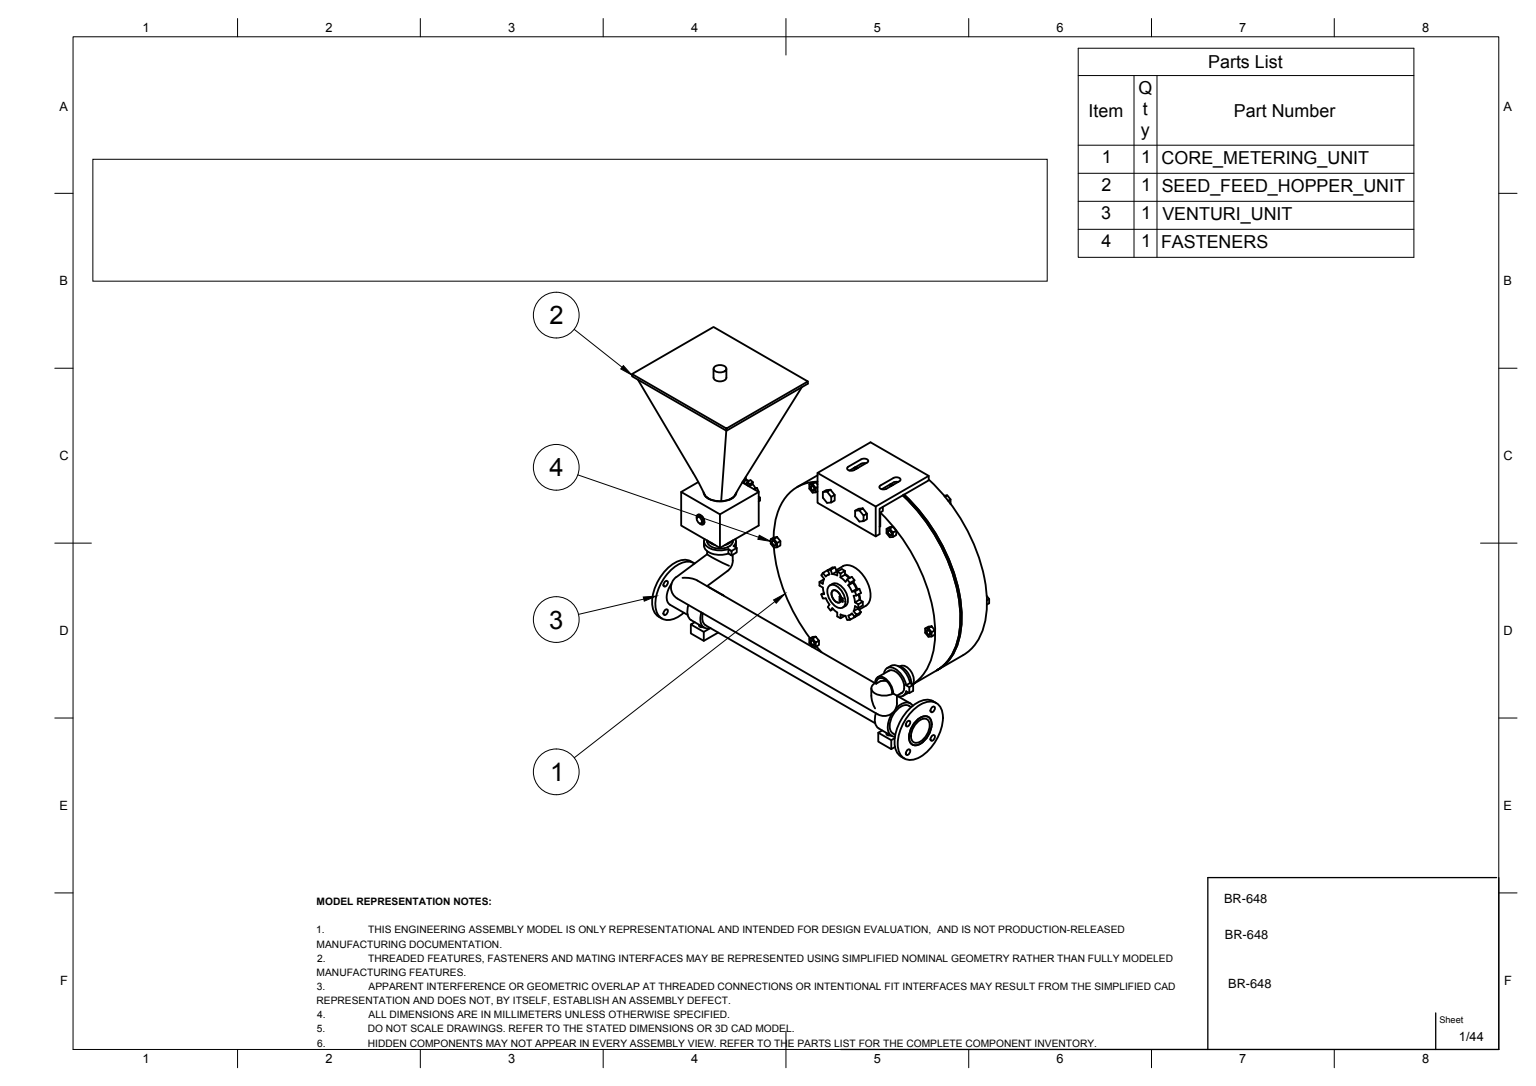
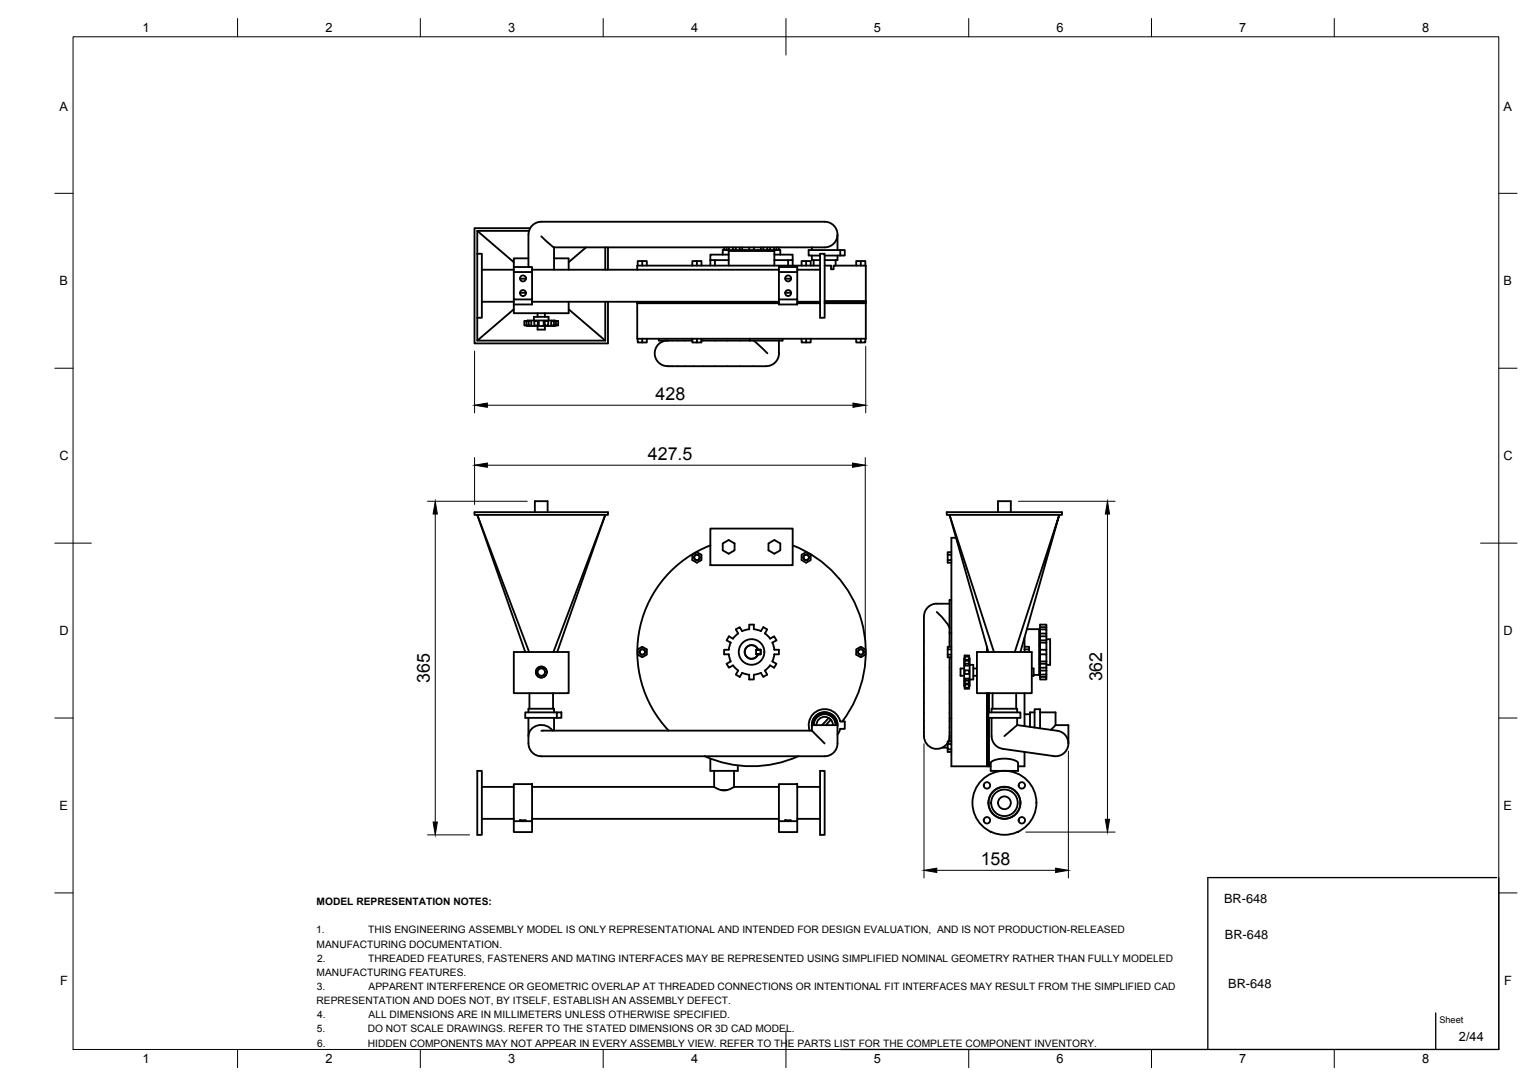
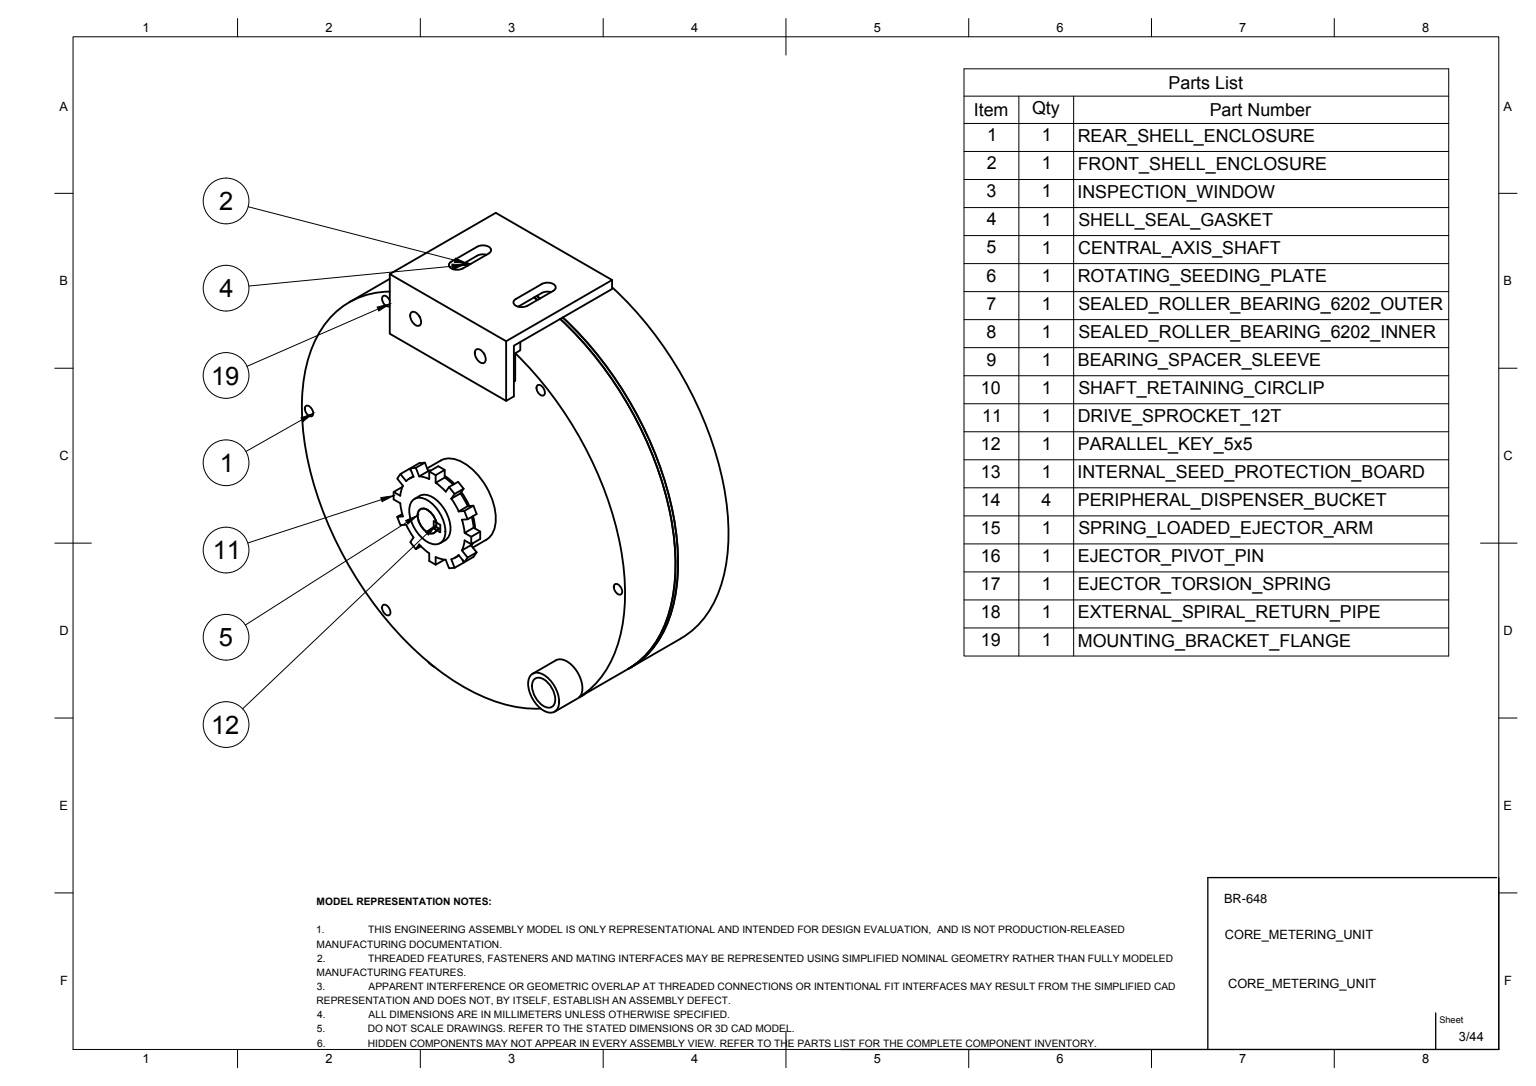
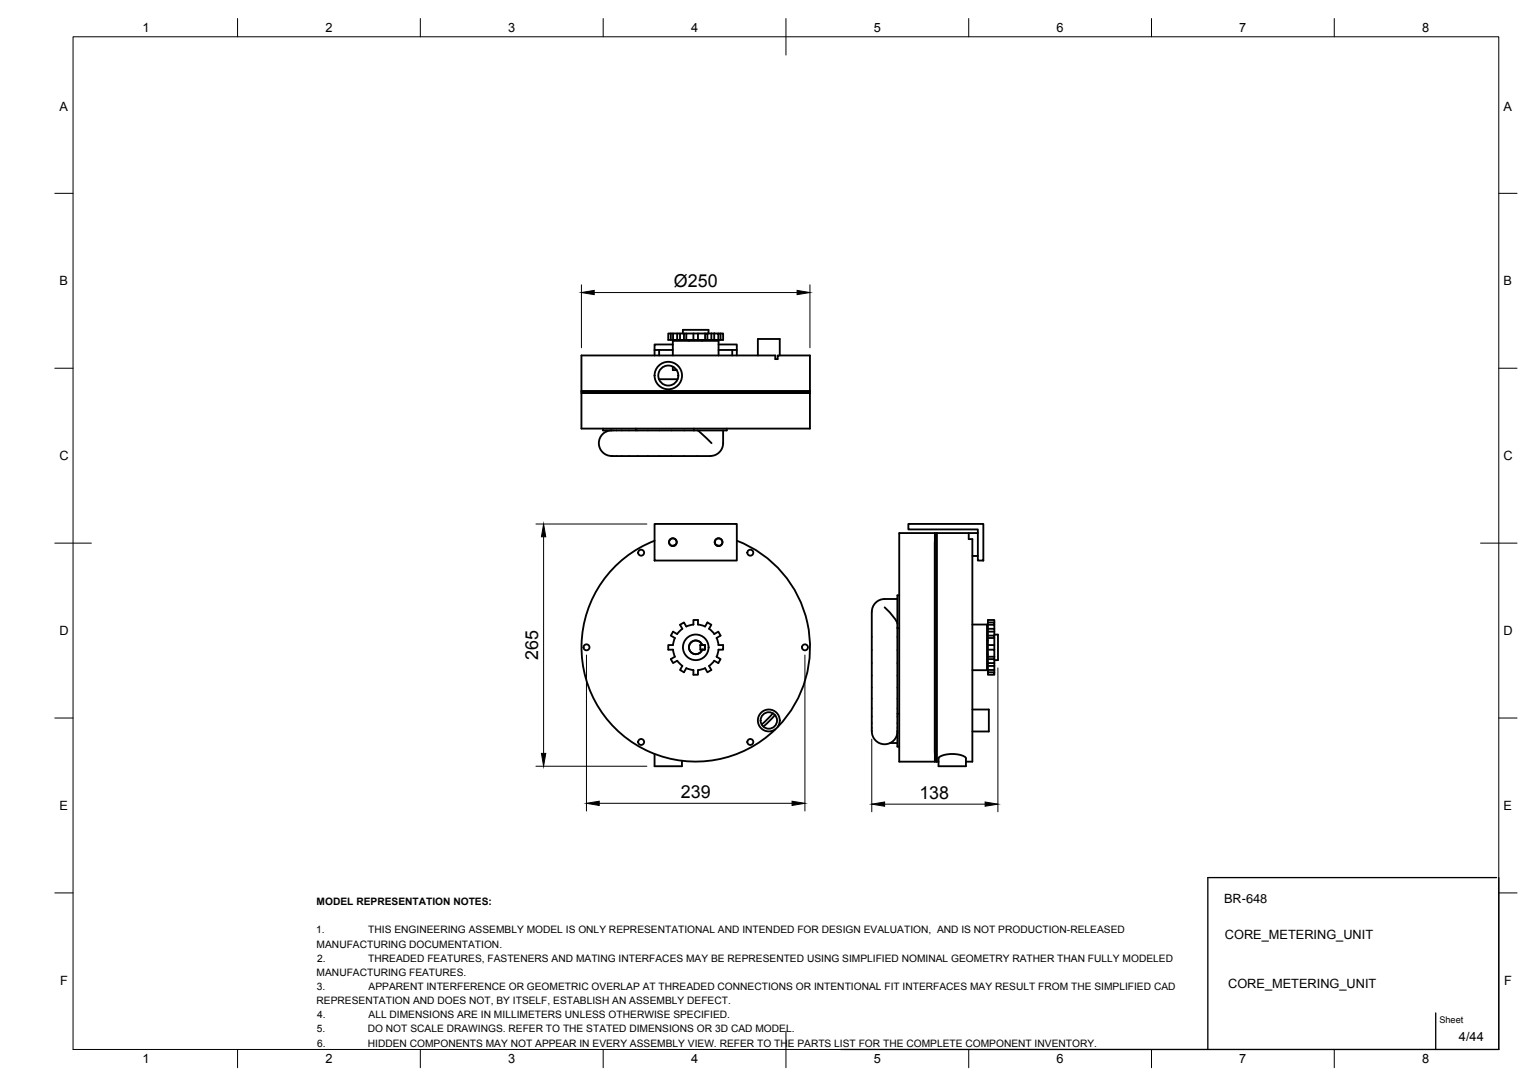
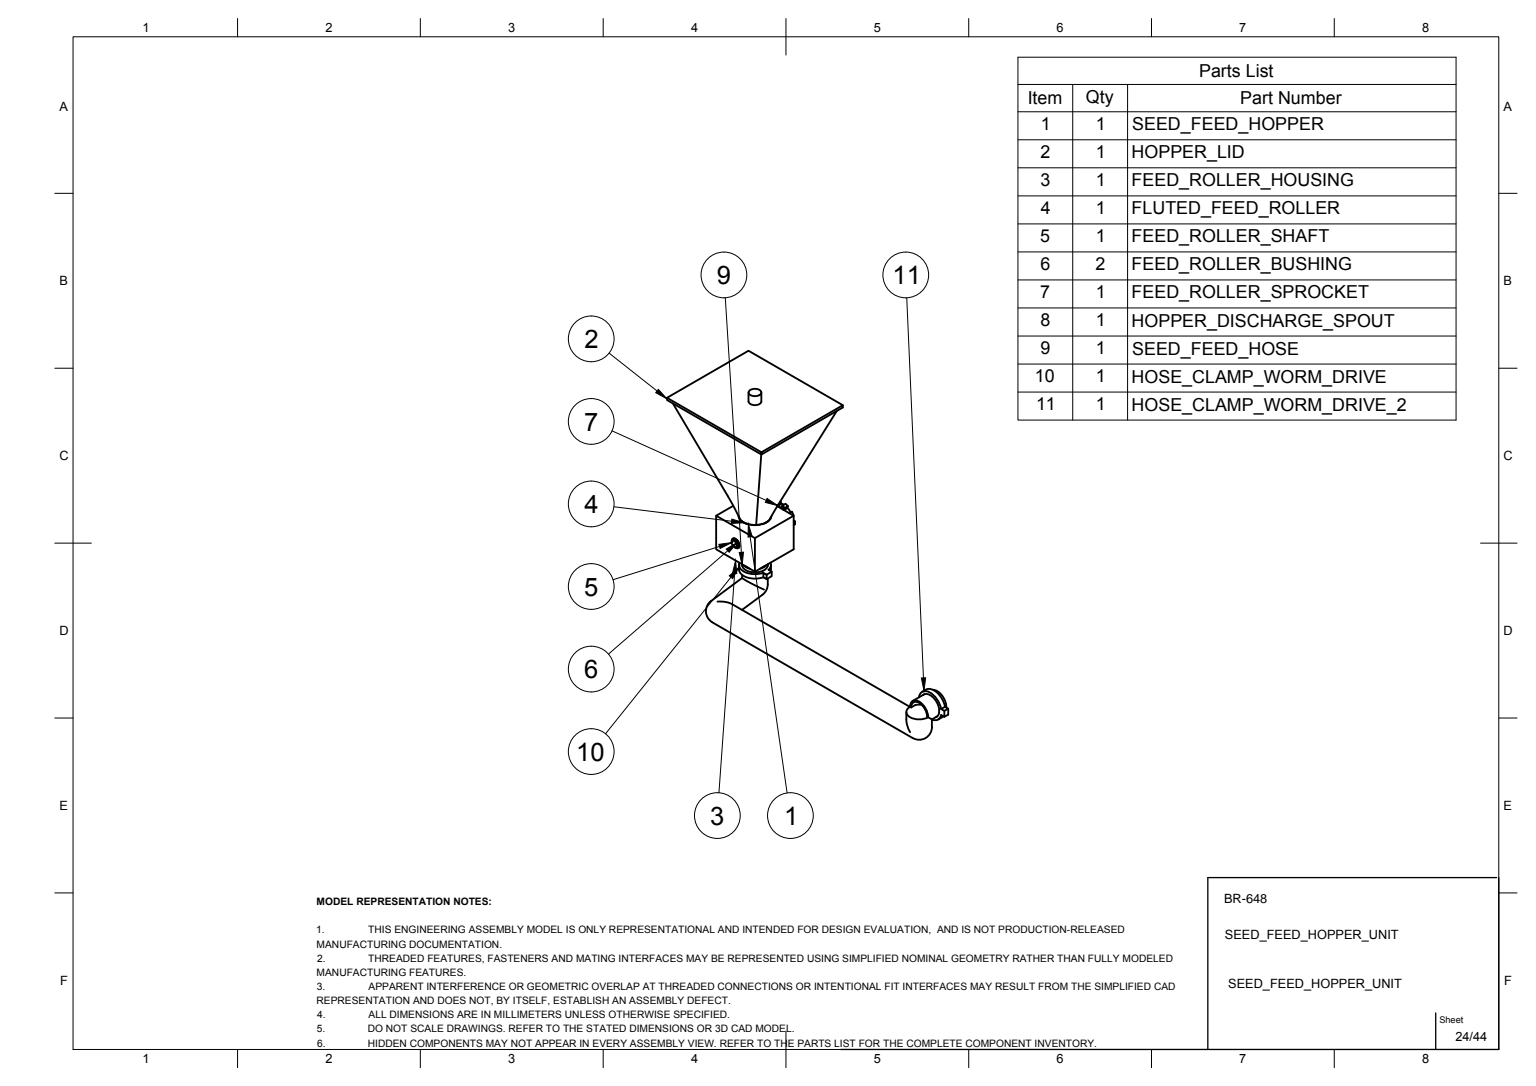
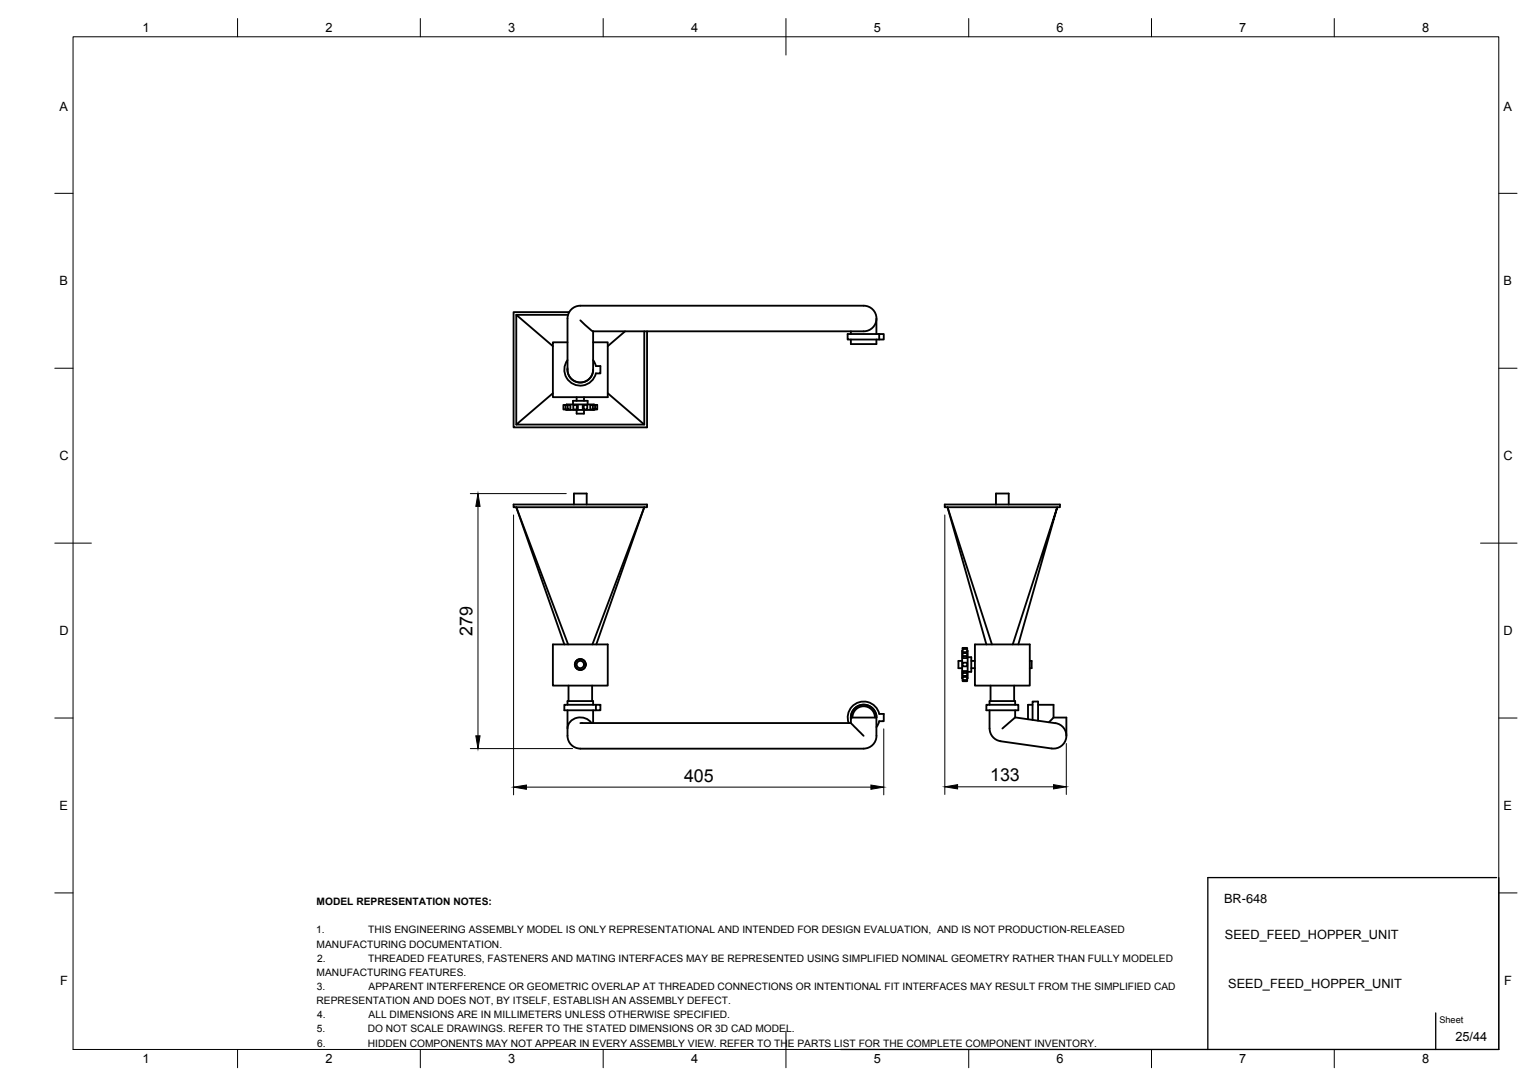
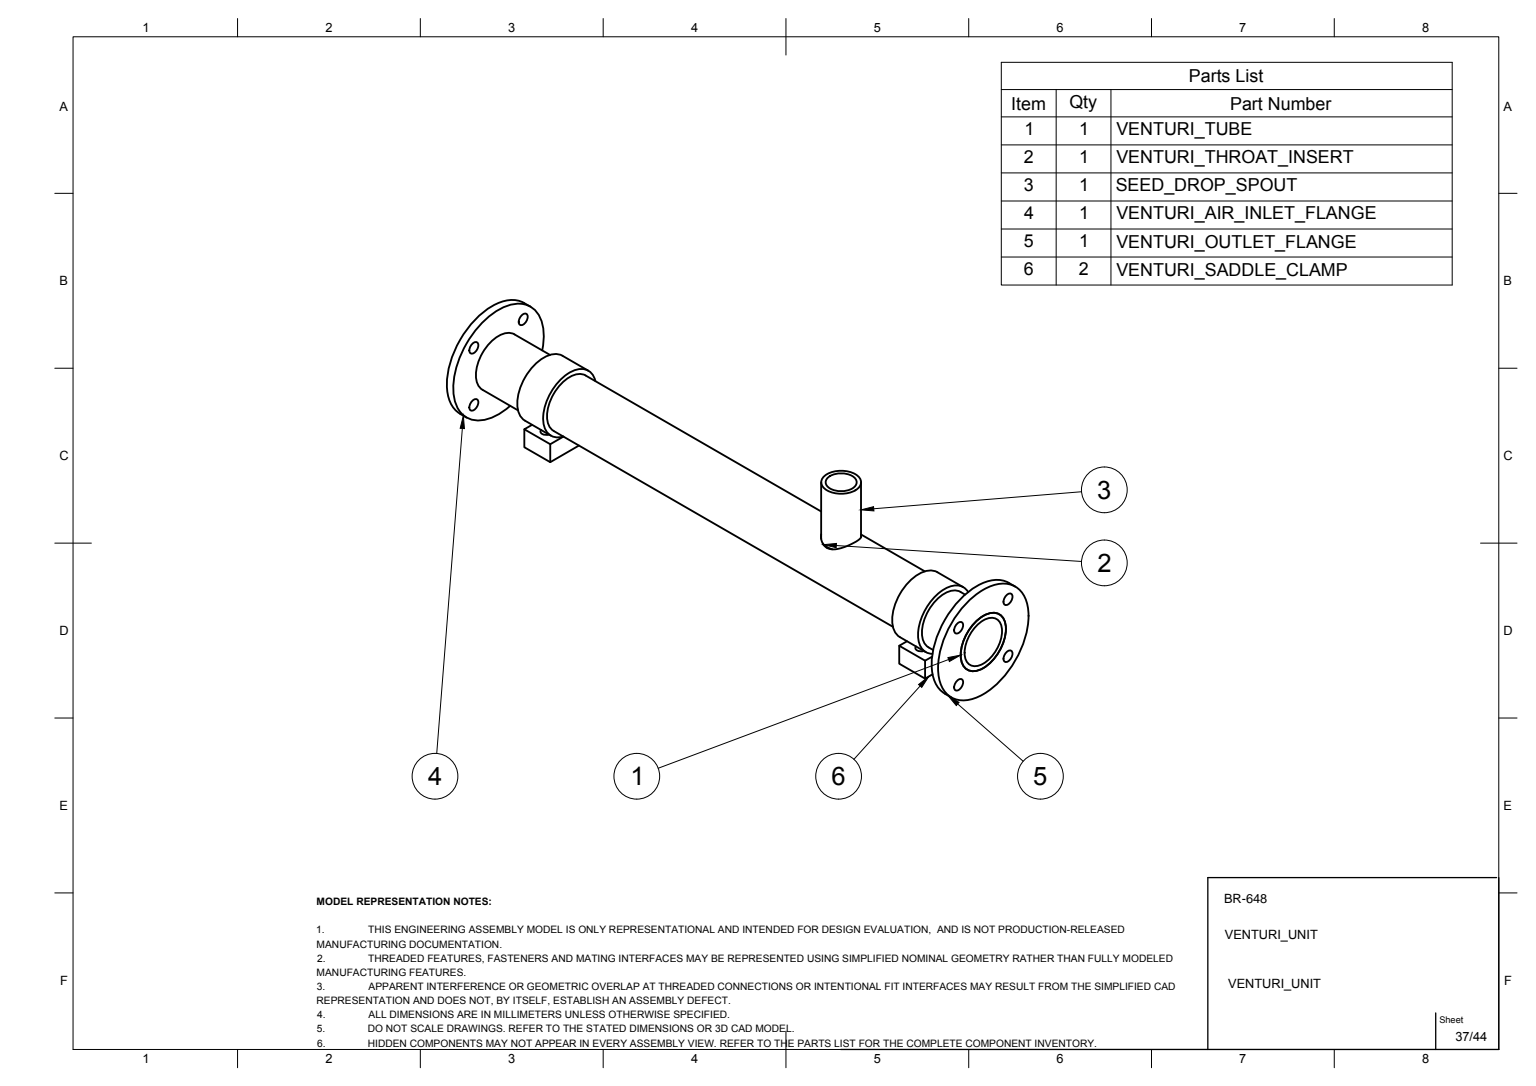
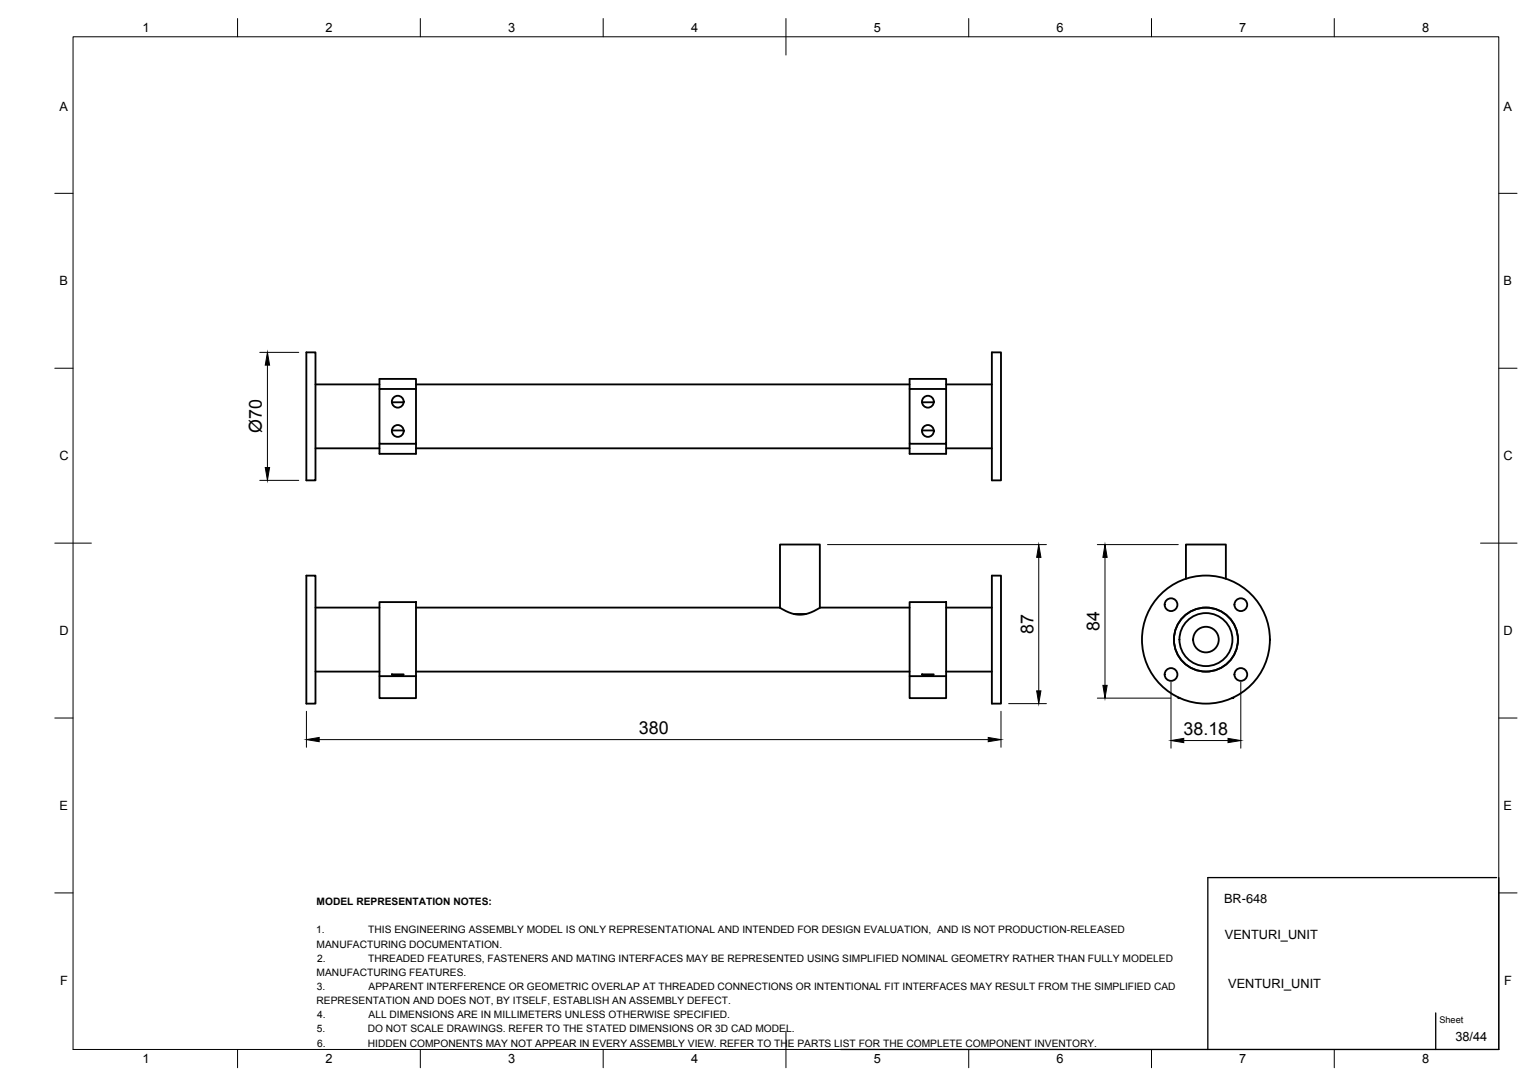
ISO-10303-21;
HEADER;
FILE_DESCRIPTION((''),'2;1');
FILE_NAME('BR-648','2026-10-01T22:05:39-07:00',(''),(''),'','','');
FILE_SCHEMA (('AUTOMOTIVE_DESIGN { 1 0 10303 214 3 1 1 }'));
ENDSEC;
DATA;
#10 = MECHANICAL_DESIGN_GEOMETRIC_PRESENTATION_REPRESENTATION('',(#605,#606,
#607,#608,#609,#610,#611,#612,#613,#614,#615,#616,#617,#618,#619,#620,#621,
#622,#623,#624,#625,#626,#627,#628,#629,#630,#631,#632,#633,#634,#635,#636,
#637,#638,#639,#640,#641,#642,#643,#644,#645,#646),#24628) ;
#11 = CONICAL_SURFACE('',#15204,1.225,0.221314442347791) ;
#12 = CONICAL_SURFACE('',#15210,1.225,0.221314442347791) ;
#13 = B_SPLINE_SURFACE_WITH_KNOTS('',3,3,((#22362,#22363,#22364,#22365,#22366,
#22367,#22368),(#22369,#22370,#22371,#22372,#22373,#22374,#22375),(#22376,
#22377,#22378,#22379,#22380,#22381,#22382),(#22383,#22384,#22385,#22386,
#22387,#22388,#22389),(#22390,#22391,#22392,#22393,#22394,#22395,#22396),
(#22397,#22398,#22399,#22400,#22401,#22402,#22403)),.UNSPECIFIED.,.F.,.F.,
 .F.,(4,1,1,4),(4,1,1,1,4),(-0.0016506318429804,0.2850068720673,0.571664375977581,
1.001650631843),(0.00440207412461945,0.433637210821686,0.71979396861973,
0.862872347518753,1.00595072641777),.UNSPECIFIED.) ;
#14 = B_SPLINE_SURFACE_WITH_KNOTS('',3,3,((#22475,#22476,#22477,#22478,#22479,
#22480,#22481),(#22482,#22483,#22484,#22485,#22486,#22487,#22488),(#22489,
#22490,#22491,#22492,#22493,#22494,#22495),(#22496,#22497,#22498,#22499,
#22500,#22501,#22502),(#22503,#22504,#22505,#22506,#22507,#22508,#22509),
(#22510,#22511,#22512,#22513,#22514,#22515,#22516),(#22517,#22518,#22519,
#22520,#22521,#22522,#22523)),.UNSPECIFIED.,.F.,.F.,.F.,(4,1,1,1,4),(4,
1,1,1,4),(-0.00135073644513769,0.285135398666339,0.428378466222077,0.714864601333554,
1.00135073644503),(0.00363062073752213,0.433196670488858,0.719574036989748,
0.862762720240194,1.00595140349064),.UNSPECIFIED.) ;
#15 = B_SPLINE_SURFACE_WITH_KNOTS('',3,3,((#22568,#22569,#22570,#22571,#22572,
#22573),(#22574,#22575,#22576,#22577,#22578,#22579),(#22580,#22581,#22582,
#22583,#22584,#22585),(#22586,#22587,#22588,#22589,#22590,#22591),(#22592,
#22593,#22594,#22595,#22596,#22597),(#22598,#22599,#22600,#22601,#22602,
#22603)),.UNSPECIFIED.,.F.,.F.,.F.,(4,1,1,4),(4,1,1,4),(-0.00165063184293244,
0.28500687206736,0.571664375977652,1.00165063184309),(0.00440207412461947,
0.576715589720881,0.862872347519012,1.00595072641808),.UNSPECIFIED.) ;
#16 = B_SPLINE_SURFACE_WITH_KNOTS('',3,3,((#22646,#22647,#22648,#22649,#22650,
#22651,#22652),(#22653,#22654,#22655,#22656,#22657,#22658,#22659),(#22660,
#22661,#22662,#22663,#22664,#22665,#22666),(#22667,#22668,#22669,#22670,
#22671,#22672,#22673),(#22674,#22675,#22676,#22677,#22678,#22679,#22680),
(#22681,#22682,#22683,#22684,#22685,#22686,#22687),(#22688,#22689,#22690,
#22691,#22692,#22693,#22694)),.UNSPECIFIED.,.F.,.F.,.F.,(4,1,1,1,4),(4,
1,1,1,4),(-0.00135073644515613,0.141892331110593,0.428378466222092,0.714864601333591,
1.00135073644509),(0.00363062073752213,0.433196670488988,0.719574036989965,
0.862762720240453,1.00595140349094),.UNSPECIFIED.) ;
#17 = B_SPLINE_SURFACE_WITH_KNOTS('',3,3,((#22731,#22732,#22733,#22734),(#22735,
#22736,#22737,#22738),(#22739,#22740,#22741,#22742),(#22743,#22744,#22745,
#22746),(#22747,#22748,#22749,#22750),(#22751,#22752,#22753,#22754)),
 .UNSPECIFIED.,.F.,.F.,.F.,(4,1,1,4),(4,4),(0.,0.285714285714286,0.571428571428571,
1.),(0.,1.),.UNSPECIFIED.) ;
#18 = B_SPLINE_SURFACE_WITH_KNOTS('',3,3,((#22757,#22758,#22759,#22760),(#22761,
#22762,#22763,#22764),(#22765,#22766,#22767,#22768),(#22769,#22770,#22771,
#22772),(#22773,#22774,#22775,#22776),(#22777,#22778,#22779,#22780),(#22781,
#22782,#22783,#22784)),.UNSPECIFIED.,.F.,.F.,.F.,(4,1,1,1,4),(4,4),(0.,
0.285714285714286,0.571428571428571,0.857142857142857,1.),(0.,1.),
 .UNSPECIFIED.) ;
#19 = B_SPLINE_SURFACE_WITH_KNOTS('',3,3,((#22786,#22787,#22788,#22789),(#22790,
#22791,#22792,#22793),(#22794,#22795,#22796,#22797),(#22798,#22799,#22800,
#22801),(#22802,#22803,#22804,#22805),(#22806,#22807,#22808,#22809)),
 .UNSPECIFIED.,.F.,.F.,.F.,(4,1,1,4),(4,4),(0.,0.285714285714286,0.571428571428571,
1.),(0.,1.),.UNSPECIFIED.) ;
#20 = B_SPLINE_SURFACE_WITH_KNOTS('',3,3,((#22811,#22812,#22813,#22814),(#22815,
#22816,#22817,#22818),(#22819,#22820,#22821,#22822),(#22823,#22824,#22825,
#22826),(#22827,#22828,#22829,#22830),(#22831,#22832,#22833,#22834),(#22835,
#22836,#22837,#22838)),.UNSPECIFIED.,.F.,.F.,.F.,(4,1,1,1,4),(4,4),(0.,
0.285714285714286,0.571428571428571,0.857142857142857,1.),(0.,1.),
 .UNSPECIFIED.) ;
#21 = ITEM_DEFINED_TRANSFORMATION($,$,#13654,#14833) ;
#22 = ITEM_DEFINED_TRANSFORMATION($,$,#13753,#14834) ;
#23 = ITEM_DEFINED_TRANSFORMATION($,$,#13805,#14835) ;
#24 = ITEM_DEFINED_TRANSFORMATION($,$,#13811,#14836) ;
#25 = ITEM_DEFINED_TRANSFORMATION($,$,#13838,#14837) ;
#26 = ITEM_DEFINED_TRANSFORMATION($,$,#13875,#14838) ;
#27 = ITEM_DEFINED_TRANSFORMATION($,$,#14061,#14839) ;
#28 = ITEM_DEFINED_TRANSFORMATION($,$,#14078,#14840) ;
#29 = ITEM_DEFINED_TRANSFORMATION($,$,#14095,#14841) ;
#30 = ITEM_DEFINED_TRANSFORMATION($,$,#14104,#14842) ;
#31 = ITEM_DEFINED_TRANSFORMATION($,$,#14115,#14843) ;
#32 = ITEM_DEFINED_TRANSFORMATION($,$,#14200,#14844) ;
#33 = ITEM_DEFINED_TRANSFORMATION($,$,#14207,#14845) ;
#34 = ITEM_DEFINED_TRANSFORMATION($,$,#14216,#14846) ;
#35 = ITEM_DEFINED_TRANSFORMATION($,$,#14216,#14847) ;
#36 = ITEM_DEFINED_TRANSFORMATION($,$,#14216,#14848) ;
#37 = ITEM_DEFINED_TRANSFORMATION($,$,#14216,#14849) ;
#38 = ITEM_DEFINED_TRANSFORMATION($,$,#14227,#14850) ;
#39 = ITEM_DEFINED_TRANSFORMATION($,$,#14253,#14851) ;
#40 = ITEM_DEFINED_TRANSFORMATION($,$,#14259,#14852) ;
#41 = ITEM_DEFINED_TRANSFORMATION($,$,#14495,#14853) ;
#42 = ITEM_DEFINED_TRANSFORMATION($,$,#14802,#14854) ;
#43 = ITEM_DEFINED_TRANSFORMATION($,$,#14856,#15169) ;
#44 = ITEM_DEFINED_TRANSFORMATION($,$,#14863,#15170) ;
#45 = ITEM_DEFINED_TRANSFORMATION($,$,#14884,#15171) ;
#46 = ITEM_DEFINED_TRANSFORMATION($,$,#14939,#15172) ;
#47 = ITEM_DEFINED_TRANSFORMATION($,$,#14993,#15173) ;
#48 = ITEM_DEFINED_TRANSFORMATION($,$,#14999,#15174) ;
#49 = ITEM_DEFINED_TRANSFORMATION($,$,#14999,#15175) ;
#50 = ITEM_DEFINED_TRANSFORMATION($,$,#15008,#15176) ;
#51 = ITEM_DEFINED_TRANSFORMATION($,$,#15093,#15177) ;
#52 = ITEM_DEFINED_TRANSFORMATION($,$,#15102,#15178) ;
#53 = ITEM_DEFINED_TRANSFORMATION($,$,#15143,#15179) ;
#54 = ITEM_DEFINED_TRANSFORMATION($,$,#15156,#15180) ;
#55 = ITEM_DEFINED_TRANSFORMATION($,$,#15182,#15290) ;
#56 = ITEM_DEFINED_TRANSFORMATION($,$,#15192,#15291) ;
#57 = ITEM_DEFINED_TRANSFORMATION($,$,#15213,#15292) ;
#58 = ITEM_DEFINED_TRANSFORMATION($,$,#15222,#15293) ;
#59 = ITEM_DEFINED_TRANSFORMATION($,$,#15243,#15294) ;
#60 = ITEM_DEFINED_TRANSFORMATION($,$,#15264,#15295) ;
#61 = ITEM_DEFINED_TRANSFORMATION($,$,#15264,#15296) ;
#62 = ITEM_DEFINED_TRANSFORMATION($,$,#15298,#15367) ;
#63 = ITEM_DEFINED_TRANSFORMATION($,$,#15298,#15368) ;
#64 = ITEM_DEFINED_TRANSFORMATION($,$,#15298,#15369) ;
#65 = ITEM_DEFINED_TRANSFORMATION($,$,#15308,#15370) ;
#66 = ITEM_DEFINED_TRANSFORMATION($,$,#15317,#15371) ;
#67 = ITEM_DEFINED_TRANSFORMATION($,$,#15329,#15372) ;
#68 = ITEM_DEFINED_TRANSFORMATION($,$,#15329,#15373) ;
#69 = ITEM_DEFINED_TRANSFORMATION($,$,#15342,#15374) ;
#70 = ITEM_DEFINED_TRANSFORMATION($,$,#15355,#15375) ;
#71 = ITEM_DEFINED_TRANSFORMATION($,$,#15342,#15376) ;
#72 = ITEM_DEFINED_TRANSFORMATION($,$,#15355,#15377) ;
#73 = ITEM_DEFINED_TRANSFORMATION($,$,#15342,#15378) ;
#74 = ITEM_DEFINED_TRANSFORMATION($,$,#15355,#15379) ;
#75 = ITEM_DEFINED_TRANSFORMATION($,$,#15342,#15380) ;
#76 = ITEM_DEFINED_TRANSFORMATION($,$,#15355,#15381) ;
#77 = ITEM_DEFINED_TRANSFORMATION($,$,#15342,#15382) ;
#78 = ITEM_DEFINED_TRANSFORMATION($,$,#15355,#15383) ;
#79 = ITEM_DEFINED_TRANSFORMATION($,$,#15342,#15384) ;
#80 = ITEM_DEFINED_TRANSFORMATION($,$,#15355,#15385) ;
#81 = ITEM_DEFINED_TRANSFORMATION($,$,#13653,#15386) ;
#82 = ITEM_DEFINED_TRANSFORMATION($,$,#14855,#15387) ;
#83 = ITEM_DEFINED_TRANSFORMATION($,$,#15181,#15388) ;
#84 = ITEM_DEFINED_TRANSFORMATION($,$,#15297,#15389) ;
#85 = (
REPRESENTATION_RELATIONSHIP($,$,#24793,#24792)
REPRESENTATION_RELATIONSHIP_WITH_TRANSFORMATION(#21)
SHAPE_REPRESENTATION_RELATIONSHIP()
) ;
#86 = (
REPRESENTATION_RELATIONSHIP($,$,#24794,#24792)
REPRESENTATION_RELATIONSHIP_WITH_TRANSFORMATION(#22)
SHAPE_REPRESENTATION_RELATIONSHIP()
) ;
#87 = (
REPRESENTATION_RELATIONSHIP($,$,#24795,#24792)
REPRESENTATION_RELATIONSHIP_WITH_TRANSFORMATION(#23)
SHAPE_REPRESENTATION_RELATIONSHIP()
) ;
#88 = (
REPRESENTATION_RELATIONSHIP($,$,#24796,#24792)
REPRESENTATION_RELATIONSHIP_WITH_TRANSFORMATION(#24)
SHAPE_REPRESENTATION_RELATIONSHIP()
) ;
#89 = (
REPRESENTATION_RELATIONSHIP($,$,#24797,#24792)
REPRESENTATION_RELATIONSHIP_WITH_TRANSFORMATION(#25)
SHAPE_REPRESENTATION_RELATIONSHIP()
) ;
#90 = (
REPRESENTATION_RELATIONSHIP($,$,#24798,#24792)
REPRESENTATION_RELATIONSHIP_WITH_TRANSFORMATION(#26)
SHAPE_REPRESENTATION_RELATIONSHIP()
) ;
#91 = (
REPRESENTATION_RELATIONSHIP($,$,#24799,#24792)
REPRESENTATION_RELATIONSHIP_WITH_TRANSFORMATION(#27)
SHAPE_REPRESENTATION_RELATIONSHIP()
) ;
#92 = (
REPRESENTATION_RELATIONSHIP($,$,#24800,#24792)
REPRESENTATION_RELATIONSHIP_WITH_TRANSFORMATION(#28)
SHAPE_REPRESENTATION_RELATIONSHIP()
) ;
#93 = (
REPRESENTATION_RELATIONSHIP($,$,#24801,#24792)
REPRESENTATION_RELATIONSHIP_WITH_TRANSFORMATION(#29)
SHAPE_REPRESENTATION_RELATIONSHIP()
) ;
#94 = (
REPRESENTATION_RELATIONSHIP($,$,#24802,#24792)
REPRESENTATION_RELATIONSHIP_WITH_TRANSFORMATION(#30)
SHAPE_REPRESENTATION_RELATIONSHIP()
) ;
#95 = (
REPRESENTATION_RELATIONSHIP($,$,#24803,#24792)
REPRESENTATION_RELATIONSHIP_WITH_TRANSFORMATION(#31)
SHAPE_REPRESENTATION_RELATIONSHIP()
) ;
#96 = (
REPRESENTATION_RELATIONSHIP($,$,#24804,#24792)
REPRESENTATION_RELATIONSHIP_WITH_TRANSFORMATION(#32)
SHAPE_REPRESENTATION_RELATIONSHIP()
) ;
#97 = (
REPRESENTATION_RELATIONSHIP($,$,#24805,#24792)
REPRESENTATION_RELATIONSHIP_WITH_TRANSFORMATION(#33)
SHAPE_REPRESENTATION_RELATIONSHIP()
) ;
#98 = (
REPRESENTATION_RELATIONSHIP($,$,#24806,#24792)
REPRESENTATION_RELATIONSHIP_WITH_TRANSFORMATION(#34)
SHAPE_REPRESENTATION_RELATIONSHIP()
) ;
#99 = (
REPRESENTATION_RELATIONSHIP($,$,#24806,#24792)
REPRESENTATION_RELATIONSHIP_WITH_TRANSFORMATION(#35)
SHAPE_REPRESENTATION_RELATIONSHIP()
) ;
#100 = (
REPRESENTATION_RELATIONSHIP($,$,#24806,#24792)
REPRESENTATION_RELATIONSHIP_WITH_TRANSFORMATION(#36)
SHAPE_REPRESENTATION_RELATIONSHIP()
) ;
#101 = (
REPRESENTATION_RELATIONSHIP($,$,#24806,#24792)
REPRESENTATION_RELATIONSHIP_WITH_TRANSFORMATION(#37)
SHAPE_REPRESENTATION_RELATIONSHIP()
) ;
#102 = (
REPRESENTATION_RELATIONSHIP($,$,#24807,#24792)
REPRESENTATION_RELATIONSHIP_WITH_TRANSFORMATION(#38)
SHAPE_REPRESENTATION_RELATIONSHIP()
) ;
#103 = (
REPRESENTATION_RELATIONSHIP($,$,#24808,#24792)
REPRESENTATION_RELATIONSHIP_WITH_TRANSFORMATION(#39)
SHAPE_REPRESENTATION_RELATIONSHIP()
) ;
#104 = (
REPRESENTATION_RELATIONSHIP($,$,#24809,#24792)
REPRESENTATION_RELATIONSHIP_WITH_TRANSFORMATION(#40)
SHAPE_REPRESENTATION_RELATIONSHIP()
) ;
#105 = (
REPRESENTATION_RELATIONSHIP($,$,#24810,#24792)
REPRESENTATION_RELATIONSHIP_WITH_TRANSFORMATION(#41)
SHAPE_REPRESENTATION_RELATIONSHIP()
) ;
#106 = (
REPRESENTATION_RELATIONSHIP($,$,#24811,#24792)
REPRESENTATION_RELATIONSHIP_WITH_TRANSFORMATION(#42)
SHAPE_REPRESENTATION_RELATIONSHIP()
) ;
#107 = (
REPRESENTATION_RELATIONSHIP($,$,#24813,#24812)
REPRESENTATION_RELATIONSHIP_WITH_TRANSFORMATION(#43)
SHAPE_REPRESENTATION_RELATIONSHIP()
) ;
#108 = (
REPRESENTATION_RELATIONSHIP($,$,#24814,#24812)
REPRESENTATION_RELATIONSHIP_WITH_TRANSFORMATION(#44)
SHAPE_REPRESENTATION_RELATIONSHIP()
) ;
#109 = (
REPRESENTATION_RELATIONSHIP($,$,#24815,#24812)
REPRESENTATION_RELATIONSHIP_WITH_TRANSFORMATION(#45)
SHAPE_REPRESENTATION_RELATIONSHIP()
) ;
#110 = (
REPRESENTATION_RELATIONSHIP($,$,#24816,#24812)
REPRESENTATION_RELATIONSHIP_WITH_TRANSFORMATION(#46)
SHAPE_REPRESENTATION_RELATIONSHIP()
) ;
#111 = (
REPRESENTATION_RELATIONSHIP($,$,#24817,#24812)
REPRESENTATION_RELATIONSHIP_WITH_TRANSFORMATION(#47)
SHAPE_REPRESENTATION_RELATIONSHIP()
) ;
#112 = (
REPRESENTATION_RELATIONSHIP($,$,#24818,#24812)
REPRESENTATION_RELATIONSHIP_WITH_TRANSFORMATION(#48)
SHAPE_REPRESENTATION_RELATIONSHIP()
) ;
#113 = (
REPRESENTATION_RELATIONSHIP($,$,#24818,#24812)
REPRESENTATION_RELATIONSHIP_WITH_TRANSFORMATION(#49)
SHAPE_REPRESENTATION_RELATIONSHIP()
) ;
#114 = (
REPRESENTATION_RELATIONSHIP($,$,#24819,#24812)
REPRESENTATION_RELATIONSHIP_WITH_TRANSFORMATION(#50)
SHAPE_REPRESENTATION_RELATIONSHIP()
) ;
#115 = (
REPRESENTATION_RELATIONSHIP($,$,#24820,#24812)
REPRESENTATION_RELATIONSHIP_WITH_TRANSFORMATION(#51)
SHAPE_REPRESENTATION_RELATIONSHIP()
) ;
#116 = (
REPRESENTATION_RELATIONSHIP($,$,#24821,#24812)
REPRESENTATION_RELATIONSHIP_WITH_TRANSFORMATION(#52)
SHAPE_REPRESENTATION_RELATIONSHIP()
) ;
#117 = (
REPRESENTATION_RELATIONSHIP($,$,#24822,#24812)
REPRESENTATION_RELATIONSHIP_WITH_TRANSFORMATION(#53)
SHAPE_REPRESENTATION_RELATIONSHIP()
) ;
#118 = (
REPRESENTATION_RELATIONSHIP($,$,#24823,#24812)
REPRESENTATION_RELATIONSHIP_WITH_TRANSFORMATION(#54)
SHAPE_REPRESENTATION_RELATIONSHIP()
) ;
#119 = (
REPRESENTATION_RELATIONSHIP($,$,#24825,#24824)
REPRESENTATION_RELATIONSHIP_WITH_TRANSFORMATION(#55)
SHAPE_REPRESENTATION_RELATIONSHIP()
) ;
#120 = (
REPRESENTATION_RELATIONSHIP($,$,#24826,#24824)
REPRESENTATION_RELATIONSHIP_WITH_TRANSFORMATION(#56)
SHAPE_REPRESENTATION_RELATIONSHIP()
) ;
#121 = (
REPRESENTATION_RELATIONSHIP($,$,#24827,#24824)
REPRESENTATION_RELATIONSHIP_WITH_TRANSFORMATION(#57)
SHAPE_REPRESENTATION_RELATIONSHIP()
) ;
#122 = (
REPRESENTATION_RELATIONSHIP($,$,#24828,#24824)
REPRESENTATION_RELATIONSHIP_WITH_TRANSFORMATION(#58)
SHAPE_REPRESENTATION_RELATIONSHIP()
) ;
#123 = (
REPRESENTATION_RELATIONSHIP($,$,#24829,#24824)
REPRESENTATION_RELATIONSHIP_WITH_TRANSFORMATION(#59)
SHAPE_REPRESENTATION_RELATIONSHIP()
) ;
#124 = (
REPRESENTATION_RELATIONSHIP($,$,#24830,#24824)
REPRESENTATION_RELATIONSHIP_WITH_TRANSFORMATION(#60)
SHAPE_REPRESENTATION_RELATIONSHIP()
) ;
#125 = (
REPRESENTATION_RELATIONSHIP($,$,#24830,#24824)
REPRESENTATION_RELATIONSHIP_WITH_TRANSFORMATION(#61)
SHAPE_REPRESENTATION_RELATIONSHIP()
) ;
#126 = (
REPRESENTATION_RELATIONSHIP($,$,#24832,#24831)
REPRESENTATION_RELATIONSHIP_WITH_TRANSFORMATION(#62)
SHAPE_REPRESENTATION_RELATIONSHIP()
) ;
#127 = (
REPRESENTATION_RELATIONSHIP($,$,#24832,#24831)
REPRESENTATION_RELATIONSHIP_WITH_TRANSFORMATION(#63)
SHAPE_REPRESENTATION_RELATIONSHIP()
) ;
#128 = (
REPRESENTATION_RELATIONSHIP($,$,#24832,#24831)
REPRESENTATION_RELATIONSHIP_WITH_TRANSFORMATION(#64)
SHAPE_REPRESENTATION_RELATIONSHIP()
) ;
#129 = (
REPRESENTATION_RELATIONSHIP($,$,#24833,#24831)
REPRESENTATION_RELATIONSHIP_WITH_TRANSFORMATION(#65)
SHAPE_REPRESENTATION_RELATIONSHIP()
) ;
#130 = (
REPRESENTATION_RELATIONSHIP($,$,#24834,#24831)
REPRESENTATION_RELATIONSHIP_WITH_TRANSFORMATION(#66)
SHAPE_REPRESENTATION_RELATIONSHIP()
) ;
#131 = (
REPRESENTATION_RELATIONSHIP($,$,#24835,#24831)
REPRESENTATION_RELATIONSHIP_WITH_TRANSFORMATION(#67)
SHAPE_REPRESENTATION_RELATIONSHIP()
) ;
#132 = (
REPRESENTATION_RELATIONSHIP($,$,#24835,#24831)
REPRESENTATION_RELATIONSHIP_WITH_TRANSFORMATION(#68)
SHAPE_REPRESENTATION_RELATIONSHIP()
) ;
#133 = (
REPRESENTATION_RELATIONSHIP($,$,#24836,#24831)
REPRESENTATION_RELATIONSHIP_WITH_TRANSFORMATION(#69)
SHAPE_REPRESENTATION_RELATIONSHIP()
) ;
#134 = (
REPRESENTATION_RELATIONSHIP($,$,#24837,#24831)
REPRESENTATION_RELATIONSHIP_WITH_TRANSFORMATION(#70)
SHAPE_REPRESENTATION_RELATIONSHIP()
) ;
#135 = (
REPRESENTATION_RELATIONSHIP($,$,#24836,#24831)
REPRESENTATION_RELATIONSHIP_WITH_TRANSFORMATION(#71)
SHAPE_REPRESENTATION_RELATIONSHIP()
) ;
#136 = (
REPRESENTATION_RELATIONSHIP($,$,#24837,#24831)
REPRESENTATION_RELATIONSHIP_WITH_TRANSFORMATION(#72)
SHAPE_REPRESENTATION_RELATIONSHIP()
) ;
#137 = (
REPRESENTATION_RELATIONSHIP($,$,#24836,#24831)
REPRESENTATION_RELATIONSHIP_WITH_TRANSFORMATION(#73)
SHAPE_REPRESENTATION_RELATIONSHIP()
) ;
#138 = (
REPRESENTATION_RELATIONSHIP($,$,#24837,#24831)
REPRESENTATION_RELATIONSHIP_WITH_TRANSFORMATION(#74)
SHAPE_REPRESENTATION_RELATIONSHIP()
) ;
#139 = (
REPRESENTATION_RELATIONSHIP($,$,#24836,#24831)
REPRESENTATION_RELATIONSHIP_WITH_TRANSFORMATION(#75)
SHAPE_REPRESENTATION_RELATIONSHIP()
) ;
#140 = (
REPRESENTATION_RELATIONSHIP($,$,#24837,#24831)
REPRESENTATION_RELATIONSHIP_WITH_TRANSFORMATION(#76)
SHAPE_REPRESENTATION_RELATIONSHIP()
) ;
#141 = (
REPRESENTATION_RELATIONSHIP($,$,#24836,#24831)
REPRESENTATION_RELATIONSHIP_WITH_TRANSFORMATION(#77)
SHAPE_REPRESENTATION_RELATIONSHIP()
) ;
#142 = (
REPRESENTATION_RELATIONSHIP($,$,#24837,#24831)
REPRESENTATION_RELATIONSHIP_WITH_TRANSFORMATION(#78)
SHAPE_REPRESENTATION_RELATIONSHIP()
) ;
#143 = (
REPRESENTATION_RELATIONSHIP($,$,#24836,#24831)
REPRESENTATION_RELATIONSHIP_WITH_TRANSFORMATION(#79)
SHAPE_REPRESENTATION_RELATIONSHIP()
) ;
#144 = (
REPRESENTATION_RELATIONSHIP($,$,#24837,#24831)
REPRESENTATION_RELATIONSHIP_WITH_TRANSFORMATION(#80)
SHAPE_REPRESENTATION_RELATIONSHIP()
) ;
#145 = (
REPRESENTATION_RELATIONSHIP($,$,#24792,#24791)
REPRESENTATION_RELATIONSHIP_WITH_TRANSFORMATION(#81)
SHAPE_REPRESENTATION_RELATIONSHIP()
) ;
#146 = (
REPRESENTATION_RELATIONSHIP($,$,#24812,#24791)
REPRESENTATION_RELATIONSHIP_WITH_TRANSFORMATION(#82)
SHAPE_REPRESENTATION_RELATIONSHIP()
) ;
#147 = (
REPRESENTATION_RELATIONSHIP($,$,#24824,#24791)
REPRESENTATION_RELATIONSHIP_WITH_TRANSFORMATION(#83)
SHAPE_REPRESENTATION_RELATIONSHIP()
) ;
#148 = (
REPRESENTATION_RELATIONSHIP($,$,#24831,#24791)
REPRESENTATION_RELATIONSHIP_WITH_TRANSFORMATION(#84)
SHAPE_REPRESENTATION_RELATIONSHIP()
) ;
#149 = CONTEXT_DEPENDENT_SHAPE_REPRESENTATION(#85,#24701) ;
#150 = CONTEXT_DEPENDENT_SHAPE_REPRESENTATION(#86,#24702) ;
#151 = CONTEXT_DEPENDENT_SHAPE_REPRESENTATION(#87,#24703) ;
#152 = CONTEXT_DEPENDENT_SHAPE_REPRESENTATION(#88,#24704) ;
#153 = CONTEXT_DEPENDENT_SHAPE_REPRESENTATION(#89,#24705) ;
#154 = CONTEXT_DEPENDENT_SHAPE_REPRESENTATION(#90,#24706) ;
#155 = CONTEXT_DEPENDENT_SHAPE_REPRESENTATION(#91,#24707) ;
#156 = CONTEXT_DEPENDENT_SHAPE_REPRESENTATION(#92,#24708) ;
#157 = CONTEXT_DEPENDENT_SHAPE_REPRESENTATION(#93,#24709) ;
#158 = CONTEXT_DEPENDENT_SHAPE_REPRESENTATION(#94,#24710) ;
#159 = CONTEXT_DEPENDENT_SHAPE_REPRESENTATION(#95,#24711) ;
#160 = CONTEXT_DEPENDENT_SHAPE_REPRESENTATION(#96,#24712) ;
#161 = CONTEXT_DEPENDENT_SHAPE_REPRESENTATION(#97,#24713) ;
#162 = CONTEXT_DEPENDENT_SHAPE_REPRESENTATION(#98,#24714) ;
#163 = CONTEXT_DEPENDENT_SHAPE_REPRESENTATION(#99,#24715) ;
#164 = CONTEXT_DEPENDENT_SHAPE_REPRESENTATION(#100,#24716) ;
#165 = CONTEXT_DEPENDENT_SHAPE_REPRESENTATION(#101,#24717) ;
#166 = CONTEXT_DEPENDENT_SHAPE_REPRESENTATION(#102,#24718) ;
#167 = CONTEXT_DEPENDENT_SHAPE_REPRESENTATION(#103,#24719) ;
#168 = CONTEXT_DEPENDENT_SHAPE_REPRESENTATION(#104,#24720) ;
#169 = CONTEXT_DEPENDENT_SHAPE_REPRESENTATION(#105,#24721) ;
#170 = CONTEXT_DEPENDENT_SHAPE_REPRESENTATION(#106,#24722) ;
#171 = CONTEXT_DEPENDENT_SHAPE_REPRESENTATION(#107,#24735) ;
#172 = CONTEXT_DEPENDENT_SHAPE_REPRESENTATION(#108,#24736) ;
#173 = CONTEXT_DEPENDENT_SHAPE_REPRESENTATION(#109,#24737) ;
#174 = CONTEXT_DEPENDENT_SHAPE_REPRESENTATION(#110,#24738) ;
#175 = CONTEXT_DEPENDENT_SHAPE_REPRESENTATION(#111,#24739) ;
#176 = CONTEXT_DEPENDENT_SHAPE_REPRESENTATION(#112,#24740) ;
#177 = CONTEXT_DEPENDENT_SHAPE_REPRESENTATION(#113,#24741) ;
#178 = CONTEXT_DEPENDENT_SHAPE_REPRESENTATION(#114,#24742) ;
#179 = CONTEXT_DEPENDENT_SHAPE_REPRESENTATION(#115,#24743) ;
#180 = CONTEXT_DEPENDENT_SHAPE_REPRESENTATION(#116,#24744) ;
#181 = CONTEXT_DEPENDENT_SHAPE_REPRESENTATION(#117,#24745) ;
#182 = CONTEXT_DEPENDENT_SHAPE_REPRESENTATION(#118,#24746) ;
#183 = CONTEXT_DEPENDENT_SHAPE_REPRESENTATION(#119,#24754) ;
#184 = CONTEXT_DEPENDENT_SHAPE_REPRESENTATION(#120,#24755) ;
#185 = CONTEXT_DEPENDENT_SHAPE_REPRESENTATION(#121,#24756) ;
#186 = CONTEXT_DEPENDENT_SHAPE_REPRESENTATION(#122,#24757) ;
#187 = CONTEXT_DEPENDENT_SHAPE_REPRESENTATION(#123,#24758) ;
#188 = CONTEXT_DEPENDENT_SHAPE_REPRESENTATION(#124,#24759) ;
#189 = CONTEXT_DEPENDENT_SHAPE_REPRESENTATION(#125,#24760) ;
#190 = CONTEXT_DEPENDENT_SHAPE_REPRESENTATION(#126,#24768) ;
#191 = CONTEXT_DEPENDENT_SHAPE_REPRESENTATION(#127,#24769) ;
#192 = CONTEXT_DEPENDENT_SHAPE_REPRESENTATION(#128,#24770) ;
#193 = CONTEXT_DEPENDENT_SHAPE_REPRESENTATION(#129,#24771) ;
#194 = CONTEXT_DEPENDENT_SHAPE_REPRESENTATION(#130,#24772) ;
#195 = CONTEXT_DEPENDENT_SHAPE_REPRESENTATION(#131,#24773) ;
#196 = CONTEXT_DEPENDENT_SHAPE_REPRESENTATION(#132,#24774) ;
#197 = CONTEXT_DEPENDENT_SHAPE_REPRESENTATION(#133,#24775) ;
#198 = CONTEXT_DEPENDENT_SHAPE_REPRESENTATION(#134,#24776) ;
#199 = CONTEXT_DEPENDENT_SHAPE_REPRESENTATION(#135,#24777) ;
#200 = CONTEXT_DEPENDENT_SHAPE_REPRESENTATION(#136,#24778) ;
#201 = CONTEXT_DEPENDENT_SHAPE_REPRESENTATION(#137,#24779) ;
#202 = CONTEXT_DEPENDENT_SHAPE_REPRESENTATION(#138,#24780) ;
#203 = CONTEXT_DEPENDENT_SHAPE_REPRESENTATION(#139,#24781) ;
#204 = CONTEXT_DEPENDENT_SHAPE_REPRESENTATION(#140,#24782) ;
#205 = CONTEXT_DEPENDENT_SHAPE_REPRESENTATION(#141,#24783) ;
#206 = CONTEXT_DEPENDENT_SHAPE_REPRESENTATION(#142,#24784) ;
#207 = CONTEXT_DEPENDENT_SHAPE_REPRESENTATION(#143,#24785) ;
#208 = CONTEXT_DEPENDENT_SHAPE_REPRESENTATION(#144,#24786) ;
#209 = CONTEXT_DEPENDENT_SHAPE_REPRESENTATION(#145,#24787) ;
#210 = CONTEXT_DEPENDENT_SHAPE_REPRESENTATION(#146,#24788) ;
#211 = CONTEXT_DEPENDENT_SHAPE_REPRESENTATION(#147,#24789) ;
#212 = CONTEXT_DEPENDENT_SHAPE_REPRESENTATION(#148,#24790) ;
#213 = NEXT_ASSEMBLY_USAGE_OCCURRENCE('REAR_SHELL_ENCLOSURE:1',
'REAR_SHELL_ENCLOSURE:1','REAR_SHELL_ENCLOSURE:1',#24840,#24841,
'REAR_SHELL_ENCLOSURE:1') ;
#214 = NEXT_ASSEMBLY_USAGE_OCCURRENCE('FRONT_SHELL_ENCLOSURE:1',
'FRONT_SHELL_ENCLOSURE:1','FRONT_SHELL_ENCLOSURE:1',#24840,#24842,
'FRONT_SHELL_ENCLOSURE:1') ;
#215 = NEXT_ASSEMBLY_USAGE_OCCURRENCE('INSPECTION_WINDOW:1',
'INSPECTION_WINDOW:1','INSPECTION_WINDOW:1',#24840,#24843,
'INSPECTION_WINDOW:1') ;
#216 = NEXT_ASSEMBLY_USAGE_OCCURRENCE('SHELL_SEAL_GASKET:1',
'SHELL_SEAL_GASKET:1','SHELL_SEAL_GASKET:1',#24840,#24844,
'SHELL_SEAL_GASKET:1') ;
#217 = NEXT_ASSEMBLY_USAGE_OCCURRENCE('CENTRAL_AXIS_SHAFT:1',
'CENTRAL_AXIS_SHAFT:1','CENTRAL_AXIS_SHAFT:1',#24840,#24845,
'CENTRAL_AXIS_SHAFT:1') ;
#218 = NEXT_ASSEMBLY_USAGE_OCCURRENCE('ROTATING_SEEDING_PLATE:1',
'ROTATING_SEEDING_PLATE:1','ROTATING_SEEDING_PLATE:1',#24840,#24846,
'ROTATING_SEEDING_PLATE:1') ;
#219 = NEXT_ASSEMBLY_USAGE_OCCURRENCE(
'SEALED_ROLLER_BEARING_6202_OUTER:1',
'SEALED_ROLLER_BEARING_6202_OUTER:1',
'SEALED_ROLLER_BEARING_6202_OUTER:1',#24840,#24847,
'SEALED_ROLLER_BEARING_6202_OUTER:1') ;
#220 = NEXT_ASSEMBLY_USAGE_OCCURRENCE(
'SEALED_ROLLER_BEARING_6202_INNER:1',
'SEALED_ROLLER_BEARING_6202_INNER:1',
'SEALED_ROLLER_BEARING_6202_INNER:1',#24840,#24848,
'SEALED_ROLLER_BEARING_6202_INNER:1') ;
#221 = NEXT_ASSEMBLY_USAGE_OCCURRENCE('BEARING_SPACER_SLEEVE:1',
'BEARING_SPACER_SLEEVE:1','BEARING_SPACER_SLEEVE:1',#24840,#24849,
'BEARING_SPACER_SLEEVE:1') ;
#222 = NEXT_ASSEMBLY_USAGE_OCCURRENCE('SHAFT_RETAINING_CIRCLIP:1',
'SHAFT_RETAINING_CIRCLIP:1','SHAFT_RETAINING_CIRCLIP:1',#24840,#24850,
'SHAFT_RETAINING_CIRCLIP:1') ;
#223 = NEXT_ASSEMBLY_USAGE_OCCURRENCE('DRIVE_SPROCKET_12T:1',
'DRIVE_SPROCKET_12T:1','DRIVE_SPROCKET_12T:1',#24840,#24851,
'DRIVE_SPROCKET_12T:1') ;
#224 = NEXT_ASSEMBLY_USAGE_OCCURRENCE('PARALLEL_KEY_5x5:1',
'PARALLEL_KEY_5x5:1','PARALLEL_KEY_5x5:1',#24840,#24852,
'PARALLEL_KEY_5x5:1') ;
#225 = NEXT_ASSEMBLY_USAGE_OCCURRENCE('INTERNAL_SEED_PROTECTION_BOARD:1',
'INTERNAL_SEED_PROTECTION_BOARD:1','INTERNAL_SEED_PROTECTION_BOARD:1',#24840,
#24853,'INTERNAL_SEED_PROTECTION_BOARD:1') ;
#226 = NEXT_ASSEMBLY_USAGE_OCCURRENCE('PERIPHERAL_DISPENSER_BUCKET:1',
'PERIPHERAL_DISPENSER_BUCKET:1','PERIPHERAL_DISPENSER_BUCKET:1',#24840,
#24854,'PERIPHERAL_DISPENSER_BUCKET:1') ;
#227 = NEXT_ASSEMBLY_USAGE_OCCURRENCE('PERIPHERAL_DISPENSER_BUCKET:2',
'PERIPHERAL_DISPENSER_BUCKET:2','PERIPHERAL_DISPENSER_BUCKET:2',#24840,
#24854,'PERIPHERAL_DISPENSER_BUCKET:2') ;
#228 = NEXT_ASSEMBLY_USAGE_OCCURRENCE('PERIPHERAL_DISPENSER_BUCKET:3',
'PERIPHERAL_DISPENSER_BUCKET:3','PERIPHERAL_DISPENSER_BUCKET:3',#24840,
#24854,'PERIPHERAL_DISPENSER_BUCKET:3') ;
#229 = NEXT_ASSEMBLY_USAGE_OCCURRENCE('PERIPHERAL_DISPENSER_BUCKET:4',
'PERIPHERAL_DISPENSER_BUCKET:4','PERIPHERAL_DISPENSER_BUCKET:4',#24840,
#24854,'PERIPHERAL_DISPENSER_BUCKET:4') ;
#230 = NEXT_ASSEMBLY_USAGE_OCCURRENCE('SPRING_LOADED_EJECTOR_ARM:1',
'SPRING_LOADED_EJECTOR_ARM:1','SPRING_LOADED_EJECTOR_ARM:1',#24840,#24855,
'SPRING_LOADED_EJECTOR_ARM:1') ;
#231 = NEXT_ASSEMBLY_USAGE_OCCURRENCE('EJECTOR_PIVOT_PIN:1',
'EJECTOR_PIVOT_PIN:1','EJECTOR_PIVOT_PIN:1',#24840,#24856,
'EJECTOR_PIVOT_PIN:1') ;
#232 = NEXT_ASSEMBLY_USAGE_OCCURRENCE('EJECTOR_TORSION_SPRING:1',
'EJECTOR_TORSION_SPRING:1','EJECTOR_TORSION_SPRING:1',#24840,#24857,
'EJECTOR_TORSION_SPRING:1') ;
#233 = NEXT_ASSEMBLY_USAGE_OCCURRENCE('EXTERNAL_SPIRAL_RETURN_PIPE:1',
'EXTERNAL_SPIRAL_RETURN_PIPE:1','EXTERNAL_SPIRAL_RETURN_PIPE:1',#24840,
#24858,'EXTERNAL_SPIRAL_RETURN_PIPE:1') ;
#234 = NEXT_ASSEMBLY_USAGE_OCCURRENCE('MOUNTING_BRACKET_FLANGE:1',
'MOUNTING_BRACKET_FLANGE:1','MOUNTING_BRACKET_FLANGE:1',#24840,#24859,
'MOUNTING_BRACKET_FLANGE:1') ;
#235 = NEXT_ASSEMBLY_USAGE_OCCURRENCE('SEED_FEED_HOPPER:1',
'SEED_FEED_HOPPER:1','SEED_FEED_HOPPER:1',#24860,#24861,
'SEED_FEED_HOPPER:1') ;
#236 = NEXT_ASSEMBLY_USAGE_OCCURRENCE('HOPPER_LID:1','HOPPER_LID:1',
'HOPPER_LID:1',#24860,#24862,'HOPPER_LID:1') ;
#237 = NEXT_ASSEMBLY_USAGE_OCCURRENCE('FEED_ROLLER_HOUSING:1',
'FEED_ROLLER_HOUSING:1','FEED_ROLLER_HOUSING:1',#24860,#24863,
'FEED_ROLLER_HOUSING:1') ;
#238 = NEXT_ASSEMBLY_USAGE_OCCURRENCE('FLUTED_FEED_ROLLER:1',
'FLUTED_FEED_ROLLER:1','FLUTED_FEED_ROLLER:1',#24860,#24864,
'FLUTED_FEED_ROLLER:1') ;
#239 = NEXT_ASSEMBLY_USAGE_OCCURRENCE('FEED_ROLLER_SHAFT:1',
'FEED_ROLLER_SHAFT:1','FEED_ROLLER_SHAFT:1',#24860,#24865,
'FEED_ROLLER_SHAFT:1') ;
#240 = NEXT_ASSEMBLY_USAGE_OCCURRENCE('FEED_ROLLER_BUSHING:1',
'FEED_ROLLER_BUSHING:1','FEED_ROLLER_BUSHING:1',#24860,#24866,
'FEED_ROLLER_BUSHING:1') ;
#241 = NEXT_ASSEMBLY_USAGE_OCCURRENCE('FEED_ROLLER_BUSHING:2',
'FEED_ROLLER_BUSHING:2','FEED_ROLLER_BUSHING:2',#24860,#24866,
'FEED_ROLLER_BUSHING:2') ;
#242 = NEXT_ASSEMBLY_USAGE_OCCURRENCE('FEED_ROLLER_SPROCKET:1',
'FEED_ROLLER_SPROCKET:1','FEED_ROLLER_SPROCKET:1',#24860,#24867,
'FEED_ROLLER_SPROCKET:1') ;
#243 = NEXT_ASSEMBLY_USAGE_OCCURRENCE('HOPPER_DISCHARGE_SPOUT:1',
'HOPPER_DISCHARGE_SPOUT:1','HOPPER_DISCHARGE_SPOUT:1',#24860,#24868,
'HOPPER_DISCHARGE_SPOUT:1') ;
#244 = NEXT_ASSEMBLY_USAGE_OCCURRENCE('SEED_FEED_HOSE:1',
'SEED_FEED_HOSE:1','SEED_FEED_HOSE:1',#24860,#24869,'SEED_FEED_HOSE:1') ;
#245 = NEXT_ASSEMBLY_USAGE_OCCURRENCE('HOSE_CLAMP_WORM_DRIVE:1',
'HOSE_CLAMP_WORM_DRIVE:1','HOSE_CLAMP_WORM_DRIVE:1',#24860,#24870,
'HOSE_CLAMP_WORM_DRIVE:1') ;
#246 = NEXT_ASSEMBLY_USAGE_OCCURRENCE('HOSE_CLAMP_WORM_DRIVE_2:1',
'HOSE_CLAMP_WORM_DRIVE_2:1','HOSE_CLAMP_WORM_DRIVE_2:1',#24860,#24871,
'HOSE_CLAMP_WORM_DRIVE_2:1') ;
#247 = NEXT_ASSEMBLY_USAGE_OCCURRENCE('VENTURI_TUBE:1','VENTURI_TUBE:1',
'VENTURI_TUBE:1',#24872,#24873,'VENTURI_TUBE:1') ;
#248 = NEXT_ASSEMBLY_USAGE_OCCURRENCE('VENTURI_THROAT_INSERT:1',
'VENTURI_THROAT_INSERT:1','VENTURI_THROAT_INSERT:1',#24872,#24874,
'VENTURI_THROAT_INSERT:1') ;
#249 = NEXT_ASSEMBLY_USAGE_OCCURRENCE('SEED_DROP_SPOUT:1',
'SEED_DROP_SPOUT:1','SEED_DROP_SPOUT:1',#24872,#24875,
'SEED_DROP_SPOUT:1') ;
#250 = NEXT_ASSEMBLY_USAGE_OCCURRENCE('VENTURI_AIR_INLET_FLANGE:1',
'VENTURI_AIR_INLET_FLANGE:1','VENTURI_AIR_INLET_FLANGE:1',#24872,#24876,
'VENTURI_AIR_INLET_FLANGE:1') ;
#251 = NEXT_ASSEMBLY_USAGE_OCCURRENCE('VENTURI_OUTLET_FLANGE:1',
'VENTURI_OUTLET_FLANGE:1','VENTURI_OUTLET_FLANGE:1',#24872,#24877,
'VENTURI_OUTLET_FLANGE:1') ;
#252 = NEXT_ASSEMBLY_USAGE_OCCURRENCE('VENTURI_SADDLE_CLAMP:1',
'VENTURI_SADDLE_CLAMP:1','VENTURI_SADDLE_CLAMP:1',#24872,#24878,
'VENTURI_SADDLE_CLAMP:1') ;
#253 = NEXT_ASSEMBLY_USAGE_OCCURRENCE('VENTURI_SADDLE_CLAMP:2',
'VENTURI_SADDLE_CLAMP:2','VENTURI_SADDLE_CLAMP:2',#24872,#24878,
'VENTURI_SADDLE_CLAMP:2') ;
#254 = NEXT_ASSEMBLY_USAGE_OCCURRENCE('HUB_SCREW_M4:1','HUB_SCREW_M4:1',
'HUB_SCREW_M4:1',#24879,#24880,'HUB_SCREW_M4:1') ;
#255 = NEXT_ASSEMBLY_USAGE_OCCURRENCE('HUB_SCREW_M4:2','HUB_SCREW_M4:2',
'HUB_SCREW_M4:2',#24879,#24880,'HUB_SCREW_M4:2') ;
#256 = NEXT_ASSEMBLY_USAGE_OCCURRENCE('HUB_SCREW_M4:3','HUB_SCREW_M4:3',
'HUB_SCREW_M4:3',#24879,#24880,'HUB_SCREW_M4:3') ;
#257 = NEXT_ASSEMBLY_USAGE_OCCURRENCE('HUB_LOCK_WASHER:1',
'HUB_LOCK_WASHER:1','HUB_LOCK_WASHER:1',#24879,#24881,
'HUB_LOCK_WASHER:1') ;
#258 = NEXT_ASSEMBLY_USAGE_OCCURRENCE('HUB_LOCK_NUT_M10:1',
'HUB_LOCK_NUT_M10:1','HUB_LOCK_NUT_M10:1',#24879,#24882,
'HUB_LOCK_NUT_M10:1') ;
#259 = NEXT_ASSEMBLY_USAGE_OCCURRENCE('BRACKET_BOLT_M8x16:1',
'BRACKET_BOLT_M8x16:1','BRACKET_BOLT_M8x16:1',#24879,#24883,
'BRACKET_BOLT_M8x16:1') ;
#260 = NEXT_ASSEMBLY_USAGE_OCCURRENCE('BRACKET_BOLT_M8x16:2',
'BRACKET_BOLT_M8x16:2','BRACKET_BOLT_M8x16:2',#24879,#24883,
'BRACKET_BOLT_M8x16:2') ;
#261 = NEXT_ASSEMBLY_USAGE_OCCURRENCE('SHELL_CLAMP_BOLT_M6x85:1',
'SHELL_CLAMP_BOLT_M6x85:1','SHELL_CLAMP_BOLT_M6x85:1',#24879,#24884,
'SHELL_CLAMP_BOLT_M6x85:1') ;
#262 = NEXT_ASSEMBLY_USAGE_OCCURRENCE('SHELL_CLAMP_NUT_M6:1',
'SHELL_CLAMP_NUT_M6:1','SHELL_CLAMP_NUT_M6:1',#24879,#24885,
'SHELL_CLAMP_NUT_M6:1') ;
#263 = NEXT_ASSEMBLY_USAGE_OCCURRENCE('SHELL_CLAMP_BOLT_M6x85:2',
'SHELL_CLAMP_BOLT_M6x85:2','SHELL_CLAMP_BOLT_M6x85:2',#24879,#24884,
'SHELL_CLAMP_BOLT_M6x85:2') ;
#264 = NEXT_ASSEMBLY_USAGE_OCCURRENCE('SHELL_CLAMP_NUT_M6:2',
'SHELL_CLAMP_NUT_M6:2','SHELL_CLAMP_NUT_M6:2',#24879,#24885,
'SHELL_CLAMP_NUT_M6:2') ;
#265 = NEXT_ASSEMBLY_USAGE_OCCURRENCE('SHELL_CLAMP_BOLT_M6x85:3',
'SHELL_CLAMP_BOLT_M6x85:3','SHELL_CLAMP_BOLT_M6x85:3',#24879,#24884,
'SHELL_CLAMP_BOLT_M6x85:3') ;
#266 = NEXT_ASSEMBLY_USAGE_OCCURRENCE('SHELL_CLAMP_NUT_M6:3',
'SHELL_CLAMP_NUT_M6:3','SHELL_CLAMP_NUT_M6:3',#24879,#24885,
'SHELL_CLAMP_NUT_M6:3') ;
#267 = NEXT_ASSEMBLY_USAGE_OCCURRENCE('SHELL_CLAMP_BOLT_M6x85:4',
'SHELL_CLAMP_BOLT_M6x85:4','SHELL_CLAMP_BOLT_M6x85:4',#24879,#24884,
'SHELL_CLAMP_BOLT_M6x85:4') ;
#268 = NEXT_ASSEMBLY_USAGE_OCCURRENCE('SHELL_CLAMP_NUT_M6:4',
'SHELL_CLAMP_NUT_M6:4','SHELL_CLAMP_NUT_M6:4',#24879,#24885,
'SHELL_CLAMP_NUT_M6:4') ;
#269 = NEXT_ASSEMBLY_USAGE_OCCURRENCE('SHELL_CLAMP_BOLT_M6x85:5',
'SHELL_CLAMP_BOLT_M6x85:5','SHELL_CLAMP_BOLT_M6x85:5',#24879,#24884,
'SHELL_CLAMP_BOLT_M6x85:5') ;
#270 = NEXT_ASSEMBLY_USAGE_OCCURRENCE('SHELL_CLAMP_NUT_M6:5',
'SHELL_CLAMP_NUT_M6:5','SHELL_CLAMP_NUT_M6:5',#24879,#24885,
'SHELL_CLAMP_NUT_M6:5') ;
#271 = NEXT_ASSEMBLY_USAGE_OCCURRENCE('SHELL_CLAMP_BOLT_M6x85:6',
'SHELL_CLAMP_BOLT_M6x85:6','SHELL_CLAMP_BOLT_M6x85:6',#24879,#24884,
'SHELL_CLAMP_BOLT_M6x85:6') ;
#272 = NEXT_ASSEMBLY_USAGE_OCCURRENCE('SHELL_CLAMP_NUT_M6:6',
'SHELL_CLAMP_NUT_M6:6','SHELL_CLAMP_NUT_M6:6',#24879,#24885,
'SHELL_CLAMP_NUT_M6:6') ;
#273 = NEXT_ASSEMBLY_USAGE_OCCURRENCE('CORE_METERING_UNIT:1',
'CORE_METERING_UNIT:1','CORE_METERING_UNIT:1',#24839,#24840,
'CORE_METERING_UNIT:1') ;
#274 = NEXT_ASSEMBLY_USAGE_OCCURRENCE('SEED_FEED_HOPPER_UNIT:1',
'SEED_FEED_HOPPER_UNIT:1','SEED_FEED_HOPPER_UNIT:1',#24839,#24860,
'SEED_FEED_HOPPER_UNIT:1') ;
#275 = NEXT_ASSEMBLY_USAGE_OCCURRENCE('VENTURI_UNIT:1','VENTURI_UNIT:1',
'VENTURI_UNIT:1',#24839,#24872,'VENTURI_UNIT:1') ;
#276 = NEXT_ASSEMBLY_USAGE_OCCURRENCE('FASTENERS:1','FASTENERS:1',
'FASTENERS:1',#24839,#24879,'FASTENERS:1') ;
#277 = ELLIPSE('',#14403,0.0541051040647724,0.05) ;
#278 = ELLIPSE('',#14404,0.0541051040647724,0.05) ;
#279 = ELLIPSE('',#14405,0.0541051040647724,0.05) ;
#280 = ELLIPSE('',#14408,0.0541051040647731,0.05) ;
#281 = ELLIPSE('',#14409,0.0541051040647731,0.05) ;
#282 = ELLIPSE('',#14411,0.0541051040647723,0.05) ;
#283 = ELLIPSE('',#14413,0.0541051040647739,0.05) ;
#284 = ELLIPSE('',#14415,0.0541051040647728,0.05) ;
#285 = ELLIPSE('',#14417,0.0541051040647725,0.05) ;
#286 = ELLIPSE('',#14418,0.0541051040647725,0.05) ;
#287 = ELLIPSE('',#14420,0.0541051040647722,0.05) ;
#288 = ELLIPSE('',#14421,0.0541051040647722,0.05) ;
#289 = ELLIPSE('',#14422,0.0541051040647722,0.05) ;
#290 = ELLIPSE('',#14424,0.0541051040647732,0.05) ;
#291 = ELLIPSE('',#14425,0.0541051040647732,0.05) ;
#292 = ELLIPSE('',#14427,0.054105104064773,0.05) ;
#293 = ELLIPSE('',#14428,0.054105104064773,0.05) ;
#294 = ELLIPSE('',#14429,0.054105104064773,0.05) ;
#295 = ELLIPSE('',#14431,0.0541051040647731,0.05) ;
#296 = ELLIPSE('',#14432,0.0541051040647731,0.05) ;
#297 = ELLIPSE('',#14434,0.0541051040647723,0.05) ;
#298 = ELLIPSE('',#14436,0.0541051040647739,0.05) ;
#299 = ELLIPSE('',#14438,0.0541051040647728,0.05) ;
#300 = ELLIPSE('',#14440,0.0541051040647725,0.05) ;
#301 = ELLIPSE('',#14441,0.0541051040647725,0.05) ;
#302 = ELLIPSE('',#14443,0.0541051040647722,0.05) ;
#303 = ELLIPSE('',#14444,0.0541051040647722,0.05) ;
#304 = ELLIPSE('',#14445,0.0541051040647722,0.05) ;
#305 = ELLIPSE('',#14447,0.0541051040647732,0.05) ;
#306 = ELLIPSE('',#14448,0.0541051040647732,0.05) ;
#307 = ELLIPSE('',#14450,0.0541051040647732,0.05) ;
#308 = ELLIPSE('',#14451,0.0541051040647732,0.05) ;
#309 = ELLIPSE('',#14452,0.0541051040647732,0.05) ;
#310 = ELLIPSE('',#14454,0.0541051040647731,0.05) ;
#311 = ELLIPSE('',#14455,0.0541051040647731,0.05) ;
#312 = ELLIPSE('',#14457,0.0541051040647721,0.05) ;
#313 = ELLIPSE('',#14459,0.0541051040647739,0.05) ;
#314 = ELLIPSE('',#14461,0.0541051040647728,0.05) ;
#315 = ELLIPSE('',#14463,0.0541051040647725,0.05) ;
#316 = ELLIPSE('',#14464,0.0541051040647725,0.05) ;
#317 = ELLIPSE('',#14466,0.0541051040647719,0.05) ;
#318 = ELLIPSE('',#14467,0.0541051040647719,0.05) ;
#319 = ELLIPSE('',#14468,0.0541051040647719,0.05) ;
#320 = ELLIPSE('',#14470,0.0541051040647732,0.05) ;
#321 = ELLIPSE('',#14471,0.0541051040647732,0.05) ;
#322 = ELLIPSE('',#14473,0.0541051040647732,0.05) ;
#323 = ELLIPSE('',#14474,0.0541051040647732,0.05) ;
#324 = ELLIPSE('',#14475,0.0541051040647732,0.05) ;
#325 = ELLIPSE('',#14477,0.0541051040647731,0.05) ;
#326 = ELLIPSE('',#14478,0.0541051040647731,0.05) ;
#327 = ELLIPSE('',#14480,0.0541051040647723,0.05) ;
#328 = ELLIPSE('',#14482,0.0541051040647732,0.05) ;
#329 = ELLIPSE('',#14484,0.0541051040647732,0.05) ;
#330 = ELLIPSE('',#14486,0.0541051040647725,0.05) ;
#331 = ELLIPSE('',#14487,0.0541051040647725,0.05) ;
#332 = ELLIPSE('',#14489,0.0541051040647719,0.05) ;
#333 = ELLIPSE('',#14490,0.0541051040647719,0.05) ;
#334 = ELLIPSE('',#14491,0.0541051040647719,0.05) ;
#335 = ELLIPSE('',#14693,1.97989898732233,1.4) ;
#336 = ELLIPSE('',#14696,1.97989898732233,1.4) ;
#337 = ELLIPSE('',#14700,1.40426046148572,1.4) ;
#338 = ELLIPSE('',#14702,1.40426046148572,1.4) ;
#339 = ELLIPSE('',#14708,1.40426046148572,1.4) ;
#340 = ELLIPSE('',#14711,1.40426046148572,1.4) ;
#341 = ELLIPSE('',#14714,1.40426046148572,1.4) ;
#342 = ELLIPSE('',#14719,1.40426046148572,1.4) ;
#343 = ELLIPSE('',#14724,1.40426046148572,1.4) ;
#344 = ELLIPSE('',#14727,1.40426046148572,1.4) ;
#345 = ELLIPSE('',#14730,1.40426046148572,1.4) ;
#346 = ELLIPSE('',#14735,1.40426046148572,1.4) ;
#347 = ELLIPSE('',#14740,1.40426046148572,1.4) ;
#348 = ELLIPSE('',#14743,1.40426046148572,1.4) ;
#349 = ELLIPSE('',#14746,1.40426046148572,1.4) ;
#350 = ELLIPSE('',#14751,1.40426046148572,1.4) ;
#351 = ELLIPSE('',#14756,1.97989898732233,1.4) ;
#352 = ELLIPSE('',#14757,1.97989898732233,1.4) ;
#353 = ELLIPSE('',#15108,1.97989898732233,1.4) ;
#354 = ELLIPSE('',#15114,1.97989898732233,1.4) ;
#355 = ELLIPSE('',#15116,1.97989898732233,1.4) ;
#356 = ELLIPSE('',#15134,1.97989898732233,1.4) ;
#357 = ELLIPSE('',#15135,1.97989898732233,1.4) ;
#358 = ELLIPSE('',#15137,1.85319037744393,1.4) ;
#359 = SPHERICAL_SURFACE('',#14260,0.05) ;
#360 = SPHERICAL_SURFACE('',#14263,0.05) ;
#361 = SPHERICAL_SURFACE('',#14269,0.05) ;
#362 = SPHERICAL_SURFACE('',#14274,0.05) ;
#363 = SPHERICAL_SURFACE('',#14279,0.05) ;
#364 = SPHERICAL_SURFACE('',#14284,0.05) ;
#365 = SPHERICAL_SURFACE('',#14290,0.05) ;
#366 = SPHERICAL_SURFACE('',#14293,0.05) ;
#367 = SPHERICAL_SURFACE('',#14296,0.05) ;
#368 = SPHERICAL_SURFACE('',#14299,0.05) ;
#369 = SPHERICAL_SURFACE('',#14305,0.05) ;
#370 = SPHERICAL_SURFACE('',#14310,0.05) ;
#371 = SPHERICAL_SURFACE('',#14315,0.05) ;
#372 = SPHERICAL_SURFACE('',#14320,0.05) ;
#373 = SPHERICAL_SURFACE('',#14326,0.05) ;
#374 = SPHERICAL_SURFACE('',#14329,0.05) ;
#375 = SPHERICAL_SURFACE('',#14332,0.05) ;
#376 = SPHERICAL_SURFACE('',#14335,0.05) ;
#377 = SPHERICAL_SURFACE('',#14341,0.05) ;
#378 = SPHERICAL_SURFACE('',#14346,0.05) ;
#379 = SPHERICAL_SURFACE('',#14351,0.05) ;
#380 = SPHERICAL_SURFACE('',#14356,0.05) ;
#381 = SPHERICAL_SURFACE('',#14362,0.05) ;
#382 = SPHERICAL_SURFACE('',#14365,0.05) ;
#383 = SPHERICAL_SURFACE('',#14368,0.05) ;
#384 = SPHERICAL_SURFACE('',#14371,0.05) ;
#385 = SPHERICAL_SURFACE('',#14377,0.05) ;
#386 = SPHERICAL_SURFACE('',#14382,0.05) ;
#387 = SPHERICAL_SURFACE('',#14387,0.05) ;
#388 = SPHERICAL_SURFACE('',#14392,0.05) ;
#389 = SPHERICAL_SURFACE('',#14398,0.05) ;
#390 = SPHERICAL_SURFACE('',#14496,1.1) ;
#391 = SPHERICAL_SURFACE('',#14499,1.4) ;
#392 = SPHERICAL_SURFACE('',#14501,1.1) ;
#393 = SPHERICAL_SURFACE('',#14504,1.1) ;
#394 = SPHERICAL_SURFACE('',#14506,1.1) ;
#395 = SPHERICAL_SURFACE('',#14510,1.4) ;
#396 = SPHERICAL_SURFACE('',#14511,1.4) ;
#397 = SPHERICAL_SURFACE('',#14514,1.1) ;
#398 = SPHERICAL_SURFACE('',#14517,1.4) ;
#399 = SPHERICAL_SURFACE('',#14520,1.1) ;
#400 = SPHERICAL_SURFACE('',#14524,1.4) ;
#401 = SPHERICAL_SURFACE('',#14526,1.4) ;
#402 = SPHERICAL_SURFACE('',#14528,1.1) ;
#403 = SPHERICAL_SURFACE('',#14531,1.1) ;
#404 = SPHERICAL_SURFACE('',#14533,1.4) ;
#405 = SPHERICAL_SURFACE('',#14536,1.1) ;
#406 = SPHERICAL_SURFACE('',#14539,1.4) ;
#407 = SPHERICAL_SURFACE('',#14541,1.1) ;
#408 = SPHERICAL_SURFACE('',#14545,1.4) ;
#409 = SPHERICAL_SURFACE('',#14547,1.4) ;
#410 = SPHERICAL_SURFACE('',#14549,1.1) ;
#411 = SPHERICAL_SURFACE('',#14552,1.1) ;
#412 = SPHERICAL_SURFACE('',#14554,1.4) ;
#413 = SPHERICAL_SURFACE('',#14557,1.1) ;
#414 = SPHERICAL_SURFACE('',#14560,1.4) ;
#415 = SPHERICAL_SURFACE('',#14562,1.1) ;
#416 = SPHERICAL_SURFACE('',#14566,1.4) ;
#417 = SPHERICAL_SURFACE('',#14568,1.4) ;
#418 = SPHERICAL_SURFACE('',#14570,1.1) ;
#419 = SPHERICAL_SURFACE('',#14573,1.1) ;
#420 = SPHERICAL_SURFACE('',#14575,1.4) ;
#421 = SPHERICAL_SURFACE('',#14578,1.1) ;
#422 = SPHERICAL_SURFACE('',#14581,1.4) ;
#423 = SPHERICAL_SURFACE('',#14583,1.1) ;
#424 = SPHERICAL_SURFACE('',#14587,1.4) ;
#425 = SPHERICAL_SURFACE('',#14589,1.4) ;
#426 = SPHERICAL_SURFACE('',#14590,1.1) ;
#427 = SPHERICAL_SURFACE('',#14592,1.1) ;
#428 = SPHERICAL_SURFACE('',#14593,1.4) ;
#429 = SPHERICAL_SURFACE('',#14595,1.1) ;
#430 = SPHERICAL_SURFACE('',#14598,1.4) ;
#431 = SPHERICAL_SURFACE('',#14599,1.1) ;
#432 = SPHERICAL_SURFACE('',#14603,1.4) ;
#433 = SPHERICAL_SURFACE('',#14604,1.4) ;
#434 = SPHERICAL_SURFACE('',#14605,1.1) ;
#435 = SPHERICAL_SURFACE('',#14607,1.1) ;
#436 = SPHERICAL_SURFACE('',#14608,1.4) ;
#437 = SPHERICAL_SURFACE('',#14610,1.1) ;
#438 = SPHERICAL_SURFACE('',#14615,1.4) ;
#439 = SPHERICAL_SURFACE('',#14616,1.1) ;
#440 = SPHERICAL_SURFACE('',#14622,1.4) ;
#441 = SPHERICAL_SURFACE('',#14623,1.4) ;
#442 = SPHERICAL_SURFACE('',#14624,1.1) ;
#443 = SPHERICAL_SURFACE('',#14626,1.1) ;
#444 = SPHERICAL_SURFACE('',#14627,1.4) ;
#445 = SPHERICAL_SURFACE('',#14631,1.1) ;
#446 = SPHERICAL_SURFACE('',#14632,1.1) ;
#447 = SPHERICAL_SURFACE('',#14634,1.1) ;
#448 = SPHERICAL_SURFACE('',#14635,1.4) ;
#449 = SPHERICAL_SURFACE('',#14638,1.1) ;
#450 = SPHERICAL_SURFACE('',#14641,1.4) ;
#451 = SPHERICAL_SURFACE('',#14644,1.1) ;
#452 = SPHERICAL_SURFACE('',#14650,1.4) ;
#453 = SPHERICAL_SURFACE('',#14651,1.4) ;
#454 = SPHERICAL_SURFACE('',#14656,1.4) ;
#455 = SPHERICAL_SURFACE('',#14661,1.4) ;
#456 = SPHERICAL_SURFACE('',#14666,1.4) ;
#457 = SPHERICAL_SURFACE('',#14671,1.4) ;
#458 = SPHERICAL_SURFACE('',#14676,1.4) ;
#459 = SPHERICAL_SURFACE('',#14681,1.4) ;
#460 = SPHERICAL_SURFACE('',#14684,1.4) ;
#461 = SPHERICAL_SURFACE('',#14763,1.4) ;
#462 = SPHERICAL_SURFACE('',#14764,1.4) ;
#463 = SPHERICAL_SURFACE('',#14765,1.4) ;
#464 = SPHERICAL_SURFACE('',#14766,1.4) ;
#465 = SPHERICAL_SURFACE('',#14767,1.4) ;
#466 = SPHERICAL_SURFACE('',#14768,1.4) ;
#467 = SPHERICAL_SURFACE('',#14769,1.4) ;
#468 = SPHERICAL_SURFACE('',#14773,1.4) ;
#469 = SPHERICAL_SURFACE('',#14775,1.4) ;
#470 = SPHERICAL_SURFACE('',#14776,1.1) ;
#471 = SPHERICAL_SURFACE('',#14778,1.1) ;
#472 = SPHERICAL_SURFACE('',#14779,1.1) ;
#473 = SPHERICAL_SURFACE('',#14781,1.1) ;
#474 = SPHERICAL_SURFACE('',#14782,1.1) ;
#475 = SPHERICAL_SURFACE('',#14785,1.1) ;
#476 = SPHERICAL_SURFACE('',#14787,1.1) ;
#477 = SPHERICAL_SURFACE('',#14790,1.1) ;
#478 = SPHERICAL_SURFACE('',#14792,1.1) ;
#479 = SPHERICAL_SURFACE('',#14795,1.1) ;
#480 = SPHERICAL_SURFACE('',#14797,1.1) ;
#481 = SPHERICAL_SURFACE('',#14800,1.1) ;
#482 = SPHERICAL_SURFACE('',#15121,1.4) ;
#483 = SPHERICAL_SURFACE('',#15123,1.4) ;
#484 = SPHERICAL_SURFACE('',#15129,1.4) ;
#485 = ORIENTED_CLOSED_SHELL('',*,#13120,.F.) ;
#486 = ORIENTED_CLOSED_SHELL('',*,#13122,.F.) ;
#487 = ORIENTED_CLOSED_SHELL('',*,#13133,.F.) ;
#488 = ORIENTED_CLOSED_SHELL('',*,#13134,.F.) ;
#489 = ORIENTED_CLOSED_SHELL('',*,#13135,.F.) ;
#490 = ORIENTED_CLOSED_SHELL('',*,#13136,.F.) ;
#491 = ORIENTED_CLOSED_SHELL('',*,#13137,.F.) ;
#492 = ORIENTED_CLOSED_SHELL('',*,#13138,.F.) ;
#493 = ORIENTED_CLOSED_SHELL('',*,#13139,.F.) ;
#494 = ORIENTED_CLOSED_SHELL('',*,#13140,.F.) ;
#495 = ORIENTED_CLOSED_SHELL('',*,#13141,.F.) ;
#496 = ORIENTED_CLOSED_SHELL('',*,#13142,.F.) ;
#497 = ORIENTED_CLOSED_SHELL('',*,#13143,.F.) ;
#498 = ORIENTED_CLOSED_SHELL('',*,#13144,.F.) ;
#499 = ORIENTED_CLOSED_SHELL('',*,#13145,.F.) ;
#500 = ORIENTED_CLOSED_SHELL('',*,#13146,.F.) ;
#501 = ORIENTED_CLOSED_SHELL('',*,#13147,.F.) ;
#502 = ORIENTED_CLOSED_SHELL('',*,#13148,.F.) ;
#503 = ORIENTED_CLOSED_SHELL('',*,#13149,.F.) ;
#504 = ORIENTED_CLOSED_SHELL('',*,#13150,.F.) ;
#505 = ORIENTED_CLOSED_SHELL('',*,#13151,.F.) ;
#506 = ORIENTED_CLOSED_SHELL('',*,#13152,.F.) ;
#507 = ORIENTED_CLOSED_SHELL('',*,#13153,.F.) ;
#508 = ORIENTED_CLOSED_SHELL('',*,#13154,.F.) ;
#509 = ORIENTED_CLOSED_SHELL('',*,#13155,.F.) ;
#510 = ORIENTED_CLOSED_SHELL('',*,#13156,.F.) ;
#511 = ORIENTED_CLOSED_SHELL('',*,#13157,.F.) ;
#512 = ORIENTED_CLOSED_SHELL('',*,#13159,.F.) ;
#513 = ORIENTED_CLOSED_SHELL('',*,#13160,.F.) ;
#514 = ORIENTED_CLOSED_SHELL('',*,#13161,.F.) ;
#515 = ORIENTED_CLOSED_SHELL('',*,#13162,.F.) ;
#516 = ORIENTED_CLOSED_SHELL('',*,#13163,.F.) ;
#517 = ORIENTED_CLOSED_SHELL('',*,#13164,.F.) ;
#518 = BREP_WITH_VOIDS('SEALED_ROLLER_BEARING_6202_OUTER',#13121,(#485)) ;
#519 = BREP_WITH_VOIDS('SEALED_ROLLER_BEARING_6202_INNER',#13123,(#486)) ;
#520 = BREP_WITH_VOIDS('EXTERNAL_SPIRAL_RETURN_PIPE',#13158,(#487,#488,#489,
#490,#491,#492,#493,#494,#495,#496,#497,#498,#499,#500,#501,#502,#503,#504,
#505,#506,#507,#508,#509,#510,#511,#512,#513,#514,#515,#516,#517)) ;
#521 = SHAPE_REPRESENTATION_RELATIONSHIP('SRR','None',#24793,#563) ;
#522 = SHAPE_REPRESENTATION_RELATIONSHIP('SRR','None',#24794,#564) ;
#523 = SHAPE_REPRESENTATION_RELATIONSHIP('SRR','None',#24795,#565) ;
#524 = SHAPE_REPRESENTATION_RELATIONSHIP('SRR','None',#24796,#566) ;
#525 = SHAPE_REPRESENTATION_RELATIONSHIP('SRR','None',#24797,#567) ;
#526 = SHAPE_REPRESENTATION_RELATIONSHIP('SRR','None',#24798,#568) ;
#527 = SHAPE_REPRESENTATION_RELATIONSHIP('SRR','None',#24799,#569) ;
#528 = SHAPE_REPRESENTATION_RELATIONSHIP('SRR','None',#24800,#570) ;
#529 = SHAPE_REPRESENTATION_RELATIONSHIP('SRR','None',#24801,#571) ;
#530 = SHAPE_REPRESENTATION_RELATIONSHIP('SRR','None',#24802,#572) ;
#531 = SHAPE_REPRESENTATION_RELATIONSHIP('SRR','None',#24803,#573) ;
#532 = SHAPE_REPRESENTATION_RELATIONSHIP('SRR','None',#24804,#574) ;
#533 = SHAPE_REPRESENTATION_RELATIONSHIP('SRR','None',#24805,#575) ;
#534 = SHAPE_REPRESENTATION_RELATIONSHIP('SRR','None',#24806,#576) ;
#535 = SHAPE_REPRESENTATION_RELATIONSHIP('SRR','None',#24807,#577) ;
#536 = SHAPE_REPRESENTATION_RELATIONSHIP('SRR','None',#24808,#578) ;
#537 = SHAPE_REPRESENTATION_RELATIONSHIP('SRR','None',#24809,#579) ;
#538 = SHAPE_REPRESENTATION_RELATIONSHIP('SRR','None',#24810,#580) ;
#539 = SHAPE_REPRESENTATION_RELATIONSHIP('SRR','None',#24811,#581) ;
#540 = SHAPE_REPRESENTATION_RELATIONSHIP('SRR','None',#24813,#582) ;
#541 = SHAPE_REPRESENTATION_RELATIONSHIP('SRR','None',#24814,#583) ;
#542 = SHAPE_REPRESENTATION_RELATIONSHIP('SRR','None',#24815,#584) ;
#543 = SHAPE_REPRESENTATION_RELATIONSHIP('SRR','None',#24816,#585) ;
#544 = SHAPE_REPRESENTATION_RELATIONSHIP('SRR','None',#24817,#586) ;
#545 = SHAPE_REPRESENTATION_RELATIONSHIP('SRR','None',#24818,#587) ;
#546 = SHAPE_REPRESENTATION_RELATIONSHIP('SRR','None',#24819,#588) ;
#547 = SHAPE_REPRESENTATION_RELATIONSHIP('SRR','None',#24820,#589) ;
#548 = SHAPE_REPRESENTATION_RELATIONSHIP('SRR','None',#24821,#590) ;
#549 = SHAPE_REPRESENTATION_RELATIONSHIP('SRR','None',#24822,#591) ;
#550 = SHAPE_REPRESENTATION_RELATIONSHIP('SRR','None',#24823,#592) ;
#551 = SHAPE_REPRESENTATION_RELATIONSHIP('SRR','None',#24825,#593) ;
#552 = SHAPE_REPRESENTATION_RELATIONSHIP('SRR','None',#24826,#594) ;
#553 = SHAPE_REPRESENTATION_RELATIONSHIP('SRR','None',#24827,#595) ;
#554 = SHAPE_REPRESENTATION_RELATIONSHIP('SRR','None',#24828,#596) ;
#555 = SHAPE_REPRESENTATION_RELATIONSHIP('SRR','None',#24829,#597) ;
#556 = SHAPE_REPRESENTATION_RELATIONSHIP('SRR','None',#24830,#598) ;
#557 = SHAPE_REPRESENTATION_RELATIONSHIP('SRR','None',#24832,#599) ;
#558 = SHAPE_REPRESENTATION_RELATIONSHIP('SRR','None',#24833,#600) ;
#559 = SHAPE_REPRESENTATION_RELATIONSHIP('SRR','None',#24834,#601) ;
#560 = SHAPE_REPRESENTATION_RELATIONSHIP('SRR','None',#24835,#602) ;
#561 = SHAPE_REPRESENTATION_RELATIONSHIP('SRR','None',#24836,#603) ;
#562 = SHAPE_REPRESENTATION_RELATIONSHIP('SRR','None',#24837,#604) ;
#563 = ADVANCED_BREP_SHAPE_REPRESENTATION('',(#647),#24583) ;
#564 = ADVANCED_BREP_SHAPE_REPRESENTATION('',(#648),#24584) ;
#565 = ADVANCED_BREP_SHAPE_REPRESENTATION('',(#649),#24585) ;
#566 = ADVANCED_BREP_SHAPE_REPRESENTATION('',(#650),#24586) ;
#567 = ADVANCED_BREP_SHAPE_REPRESENTATION('',(#651),#24587) ;
#568 = ADVANCED_BREP_SHAPE_REPRESENTATION('',(#652),#24588) ;
#569 = ADVANCED_BREP_SHAPE_REPRESENTATION('',(#518),#24589) ;
#570 = ADVANCED_BREP_SHAPE_REPRESENTATION('',(#519),#24590) ;
#571 = ADVANCED_BREP_SHAPE_REPRESENTATION('',(#653),#24591) ;
#572 = ADVANCED_BREP_SHAPE_REPRESENTATION('',(#654),#24592) ;
#573 = ADVANCED_BREP_SHAPE_REPRESENTATION('',(#655),#24593) ;
#574 = ADVANCED_BREP_SHAPE_REPRESENTATION('',(#656),#24594) ;
#575 = ADVANCED_BREP_SHAPE_REPRESENTATION('',(#657),#24595) ;
#576 = ADVANCED_BREP_SHAPE_REPRESENTATION('',(#658),#24596) ;
#577 = ADVANCED_BREP_SHAPE_REPRESENTATION('',(#659),#24597) ;
#578 = ADVANCED_BREP_SHAPE_REPRESENTATION('',(#660),#24598) ;
#579 = ADVANCED_BREP_SHAPE_REPRESENTATION('',(#661),#24599) ;
#580 = ADVANCED_BREP_SHAPE_REPRESENTATION('',(#520),#24600) ;
#581 = ADVANCED_BREP_SHAPE_REPRESENTATION('',(#662),#24601) ;
#582 = ADVANCED_BREP_SHAPE_REPRESENTATION('',(#663),#24603) ;
#583 = ADVANCED_BREP_SHAPE_REPRESENTATION('',(#664),#24604) ;
#584 = ADVANCED_BREP_SHAPE_REPRESENTATION('',(#665),#24605) ;
#585 = ADVANCED_BREP_SHAPE_REPRESENTATION('',(#666),#24606) ;
#586 = ADVANCED_BREP_SHAPE_REPRESENTATION('',(#667),#24607) ;
#587 = ADVANCED_BREP_SHAPE_REPRESENTATION('',(#668),#24608) ;
#588 = ADVANCED_BREP_SHAPE_REPRESENTATION('',(#669),#24609) ;
#589 = ADVANCED_BREP_SHAPE_REPRESENTATION('',(#670),#24610) ;
#590 = ADVANCED_BREP_SHAPE_REPRESENTATION('',(#671),#24611) ;
#591 = ADVANCED_BREP_SHAPE_REPRESENTATION('',(#672),#24612) ;
#592 = ADVANCED_BREP_SHAPE_REPRESENTATION('',(#673),#24613) ;
#593 = ADVANCED_BREP_SHAPE_REPRESENTATION('',(#674),#24615) ;
#594 = ADVANCED_BREP_SHAPE_REPRESENTATION('',(#675),#24616) ;
#595 = ADVANCED_BREP_SHAPE_REPRESENTATION('',(#676),#24617) ;
#596 = ADVANCED_BREP_SHAPE_REPRESENTATION('',(#677),#24618) ;
#597 = ADVANCED_BREP_SHAPE_REPRESENTATION('',(#678),#24619) ;
#598 = ADVANCED_BREP_SHAPE_REPRESENTATION('',(#679),#24620) ;
#599 = ADVANCED_BREP_SHAPE_REPRESENTATION('',(#680),#24622) ;
#600 = ADVANCED_BREP_SHAPE_REPRESENTATION('',(#681),#24623) ;
#601 = ADVANCED_BREP_SHAPE_REPRESENTATION('',(#682),#24624) ;
#602 = ADVANCED_BREP_SHAPE_REPRESENTATION('',(#683),#24625) ;
#603 = ADVANCED_BREP_SHAPE_REPRESENTATION('',(#684),#24626) ;
#604 = ADVANCED_BREP_SHAPE_REPRESENTATION('',(#685),#24627) ;
#605 = STYLED_ITEM('',(#25031),#647) ;
#606 = STYLED_ITEM('',(#25031),#648) ;
#607 = STYLED_ITEM('',(#25032),#649) ;
#608 = STYLED_ITEM('',(#25033),#650) ;
#609 = STYLED_ITEM('',(#25030),#651) ;
#610 = STYLED_ITEM('',(#25034),#652) ;
#611 = STYLED_ITEM('',(#25034),#518) ;
#612 = STYLED_ITEM('',(#25034),#519) ;
#613 = STYLED_ITEM('',(#25030),#653) ;
#614 = STYLED_ITEM('',(#25030),#654) ;
#615 = STYLED_ITEM('',(#25030),#655) ;
#616 = STYLED_ITEM('',(#25030),#656) ;
#617 = STYLED_ITEM('',(#25035),#657) ;
#618 = STYLED_ITEM('',(#25036),#658) ;
#619 = STYLED_ITEM('',(#25034),#659) ;
#620 = STYLED_ITEM('',(#25030),#660) ;
#621 = STYLED_ITEM('',(#25030),#661) ;
#622 = STYLED_ITEM('',(#25037),#520) ;
#623 = STYLED_ITEM('',(#25037),#662) ;
#624 = STYLED_ITEM('',(#25038),#663) ;
#625 = STYLED_ITEM('',(#25038),#664) ;
#626 = STYLED_ITEM('',(#25031),#665) ;
#627 = STYLED_ITEM('',(#25036),#666) ;
#628 = STYLED_ITEM('',(#25030),#667) ;
#629 = STYLED_ITEM('',(#25039),#668) ;
#630 = STYLED_ITEM('',(#25030),#669) ;
#631 = STYLED_ITEM('',(#25037),#670) ;
#632 = STYLED_ITEM('',(#25033),#671) ;
#633 = STYLED_ITEM('',(#25034),#672) ;
#634 = STYLED_ITEM('',(#25034),#673) ;
#635 = STYLED_ITEM('',(#25034),#674) ;
#636 = STYLED_ITEM('',(#25035),#675) ;
#637 = STYLED_ITEM('',(#25034),#676) ;
#638 = STYLED_ITEM('',(#25031),#677) ;
#639 = STYLED_ITEM('',(#25031),#678) ;
#640 = STYLED_ITEM('',(#25037),#679) ;
#641 = STYLED_ITEM('',(#25030),#680) ;
#642 = STYLED_ITEM('',(#25030),#681) ;
#643 = STYLED_ITEM('',(#25030),#682) ;
#644 = STYLED_ITEM('',(#25030),#683) ;
#645 = STYLED_ITEM('',(#25030),#684) ;
#646 = STYLED_ITEM('',(#25030),#685) ;
#647 = MANIFOLD_SOLID_BREP('REAR_SHELL_ENCLOSURE',#13114) ;
#648 = MANIFOLD_SOLID_BREP('FRONT_SHELL_ENCLOSURE',#13115) ;
#649 = MANIFOLD_SOLID_BREP('INSPECTION_WINDOW',#13116) ;
#650 = MANIFOLD_SOLID_BREP('SHELL_SEAL_GASKET',#13117) ;
#651 = MANIFOLD_SOLID_BREP('CENTRAL_AXIS_SHAFT',#13118) ;
#652 = MANIFOLD_SOLID_BREP('ROTATING_SEEDING_PLATE',#13119) ;
#653 = MANIFOLD_SOLID_BREP('BEARING_SPACER_SLEEVE',#13124) ;
#654 = MANIFOLD_SOLID_BREP('SHAFT_RETAINING_CIRCLIP',#13125) ;
#655 = MANIFOLD_SOLID_BREP('DRIVE_SPROCKET_12T',#13126) ;
#656 = MANIFOLD_SOLID_BREP('PARALLEL_KEY_5x5',#13127) ;
#657 = MANIFOLD_SOLID_BREP('INTERNAL_SEED_PROTECTION_BOARD',#13128) ;
#658 = MANIFOLD_SOLID_BREP('PERIPHERAL_DISPENSER_BUCKET',#13129) ;
#659 = MANIFOLD_SOLID_BREP('SPRING_LOADED_EJECTOR_ARM',#13130) ;
#660 = MANIFOLD_SOLID_BREP('EJECTOR_PIVOT_PIN',#13131) ;
#661 = MANIFOLD_SOLID_BREP('EJECTOR_TORSION_SPRING',#13132) ;
#662 = MANIFOLD_SOLID_BREP('MOUNTING_BRACKET_FLANGE',#13165) ;
#663 = MANIFOLD_SOLID_BREP('SEED_FEED_HOPPER',#13166) ;
#664 = MANIFOLD_SOLID_BREP('HOPPER_LID',#13167) ;
#665 = MANIFOLD_SOLID_BREP('FEED_ROLLER_HOUSING',#13168) ;
#666 = MANIFOLD_SOLID_BREP('FLUTED_FEED_ROLLER',#13169) ;
#667 = MANIFOLD_SOLID_BREP('FEED_ROLLER_SHAFT',#13170) ;
#668 = MANIFOLD_SOLID_BREP('FEED_ROLLER_BUSHING',#13171) ;
#669 = MANIFOLD_SOLID_BREP('FEED_ROLLER_SPROCKET',#13172) ;
#670 = MANIFOLD_SOLID_BREP('HOPPER_DISCHARGE_SPOUT',#13173) ;
#671 = MANIFOLD_SOLID_BREP('SEED_FEED_HOSE',#13174) ;
#672 = MANIFOLD_SOLID_BREP('HOSE_CLAMP_WORM_DRIVE',#13175) ;
#673 = MANIFOLD_SOLID_BREP('HOSE_CLAMP_WORM_DRIVE_2',#13176) ;
#674 = MANIFOLD_SOLID_BREP('VENTURI_TUBE',#13177) ;
#675 = MANIFOLD_SOLID_BREP('VENTURI_THROAT_INSERT',#13178) ;
#676 = MANIFOLD_SOLID_BREP('SEED_DROP_SPOUT',#13179) ;
#677 = MANIFOLD_SOLID_BREP('VENTURI_AIR_INLET_FLANGE',#13180) ;
#678 = MANIFOLD_SOLID_BREP('VENTURI_OUTLET_FLANGE',#13181) ;
#679 = MANIFOLD_SOLID_BREP('VENTURI_SADDLE_CLAMP',#13182) ;
#680 = MANIFOLD_SOLID_BREP('HUB_SCREW_M4',#13183) ;
#681 = MANIFOLD_SOLID_BREP('HUB_LOCK_WASHER',#13184) ;
#682 = MANIFOLD_SOLID_BREP('HUB_LOCK_NUT_M10',#13185) ;
#683 = MANIFOLD_SOLID_BREP('BRACKET_BOLT_M8x16',#13186) ;
#684 = MANIFOLD_SOLID_BREP('SHELL_CLAMP_BOLT_M6x85',#13187) ;
#685 = MANIFOLD_SOLID_BREP('SHELL_CLAMP_NUT_M6',#13188) ;
#686 = FACE_BOUND('',#3722,.T.) ;
#687 = FACE_BOUND('',#3726,.T.) ;
#688 = FACE_BOUND('',#3738,.T.) ;
#689 = FACE_BOUND('',#3739,.T.) ;
#690 = FACE_BOUND('',#3743,.T.) ;
#691 = FACE_BOUND('',#3748,.T.) ;
#692 = FACE_BOUND('',#3755,.T.) ;
#693 = FACE_BOUND('',#3757,.T.) ;
#694 = FACE_BOUND('',#3758,.T.) ;
#695 = FACE_BOUND('',#3759,.T.) ;
#696 = FACE_BOUND('',#3760,.T.) ;
#697 = FACE_BOUND('',#3761,.T.) ;
#698 = FACE_BOUND('',#3762,.T.) ;
#699 = FACE_BOUND('',#3763,.T.) ;
#700 = FACE_BOUND('',#3767,.T.) ;
#701 = FACE_BOUND('',#3770,.T.) ;
#702 = FACE_BOUND('',#3773,.T.) ;
#703 = FACE_BOUND('',#3776,.T.) ;
#704 = FACE_BOUND('',#3778,.T.) ;
#705 = FACE_BOUND('',#3779,.T.) ;
#706 = FACE_BOUND('',#3780,.T.) ;
#707 = FACE_BOUND('',#3781,.T.) ;
#708 = FACE_BOUND('',#3782,.T.) ;
#709 = FACE_BOUND('',#3783,.T.) ;
#710 = FACE_BOUND('',#3784,.T.) ;
#711 = FACE_BOUND('',#3795,.T.) ;
#712 = FACE_BOUND('',#3799,.T.) ;
#713 = FACE_BOUND('',#3802,.T.) ;
#714 = FACE_BOUND('',#3806,.T.) ;
#715 = FACE_BOUND('',#3807,.T.) ;
#716 = FACE_BOUND('',#3808,.T.) ;
#717 = FACE_BOUND('',#3809,.T.) ;
#718 = FACE_BOUND('',#3812,.T.) ;
#719 = FACE_BOUND('',#3813,.T.) ;
#720 = FACE_BOUND('',#3814,.T.) ;
#721 = FACE_BOUND('',#3815,.T.) ;
#722 = FACE_BOUND('',#3816,.T.) ;
#723 = FACE_BOUND('',#3817,.T.) ;
#724 = FACE_BOUND('',#3818,.T.) ;
#725 = FACE_BOUND('',#3820,.T.) ;
#726 = FACE_BOUND('',#3821,.T.) ;
#727 = FACE_BOUND('',#3822,.T.) ;
#728 = FACE_BOUND('',#3823,.T.) ;
#729 = FACE_BOUND('',#3824,.T.) ;
#730 = FACE_BOUND('',#3825,.T.) ;
#731 = FACE_BOUND('',#3826,.T.) ;
#732 = FACE_BOUND('',#3827,.T.) ;
#733 = FACE_BOUND('',#3828,.T.) ;
#734 = FACE_BOUND('',#3829,.T.) ;
#735 = FACE_BOUND('',#3842,.T.) ;
#736 = FACE_BOUND('',#3843,.T.) ;
#737 = FACE_BOUND('',#3844,.T.) ;
#738 = FACE_BOUND('',#3845,.T.) ;
#739 = FACE_BOUND('',#3846,.T.) ;
#740 = FACE_BOUND('',#3847,.T.) ;
#741 = FACE_BOUND('',#3848,.T.) ;
#742 = FACE_BOUND('',#3850,.T.) ;
#743 = FACE_BOUND('',#3851,.T.) ;
#744 = FACE_BOUND('',#3852,.T.) ;
#745 = FACE_BOUND('',#3853,.T.) ;
#746 = FACE_BOUND('',#3854,.T.) ;
#747 = FACE_BOUND('',#3855,.T.) ;
#748 = FACE_BOUND('',#3856,.T.) ;
#749 = FACE_BOUND('',#3864,.T.) ;
#750 = FACE_BOUND('',#3866,.T.) ;
#751 = FACE_BOUND('',#3872,.T.) ;
#752 = FACE_BOUND('',#3873,.T.) ;
#753 = FACE_BOUND('',#3874,.T.) ;
#754 = FACE_BOUND('',#3875,.T.) ;
#755 = FACE_BOUND('',#3881,.T.) ;
#756 = FACE_BOUND('',#3882,.T.) ;
#757 = FACE_BOUND('',#3883,.T.) ;
#758 = FACE_BOUND('',#3884,.T.) ;
#759 = FACE_BOUND('',#3963,.T.) ;
#760 = FACE_BOUND('',#3964,.T.) ;
#761 = FACE_BOUND('',#3965,.T.) ;
#762 = FACE_BOUND('',#3966,.T.) ;
#763 = FACE_BOUND('',#3967,.T.) ;
#764 = FACE_BOUND('',#3968,.T.) ;
#765 = FACE_BOUND('',#3969,.T.) ;
#766 = FACE_BOUND('',#3970,.T.) ;
#767 = FACE_BOUND('',#3971,.T.) ;
#768 = FACE_BOUND('',#3972,.T.) ;
#769 = FACE_BOUND('',#3973,.T.) ;
#770 = FACE_BOUND('',#3974,.T.) ;
#771 = FACE_BOUND('',#3975,.T.) ;
#772 = FACE_BOUND('',#3976,.T.) ;
#773 = FACE_BOUND('',#3977,.T.) ;
#774 = FACE_BOUND('',#3978,.T.) ;
#775 = FACE_BOUND('',#3979,.T.) ;
#776 = FACE_BOUND('',#3980,.T.) ;
#777 = FACE_BOUND('',#3981,.T.) ;
#778 = FACE_BOUND('',#3982,.T.) ;
#779 = FACE_BOUND('',#3983,.T.) ;
#780 = FACE_BOUND('',#3984,.T.) ;
#781 = FACE_BOUND('',#3985,.T.) ;
#782 = FACE_BOUND('',#3986,.T.) ;
#783 = FACE_BOUND('',#3987,.T.) ;
#784 = FACE_BOUND('',#3988,.T.) ;
#785 = FACE_BOUND('',#3989,.T.) ;
#786 = FACE_BOUND('',#3990,.T.) ;
#787 = FACE_BOUND('',#3991,.T.) ;
#788 = FACE_BOUND('',#3992,.T.) ;
#789 = FACE_BOUND('',#3993,.T.) ;
#790 = FACE_BOUND('',#3994,.T.) ;
#791 = FACE_BOUND('',#3995,.T.) ;
#792 = FACE_BOUND('',#3996,.T.) ;
#793 = FACE_BOUND('',#3997,.T.) ;
#794 = FACE_BOUND('',#3998,.T.) ;
#795 = FACE_BOUND('',#3999,.T.) ;
#796 = FACE_BOUND('',#4000,.T.) ;
#797 = FACE_BOUND('',#4001,.T.) ;
#798 = FACE_BOUND('',#4002,.T.) ;
#799 = FACE_BOUND('',#4003,.T.) ;
#800 = FACE_BOUND('',#4004,.T.) ;
#801 = FACE_BOUND('',#4005,.T.) ;
#802 = FACE_BOUND('',#4006,.T.) ;
#803 = FACE_BOUND('',#4007,.T.) ;
#804 = FACE_BOUND('',#4008,.T.) ;
#805 = FACE_BOUND('',#4009,.T.) ;
#806 = FACE_BOUND('',#4010,.T.) ;
#807 = FACE_BOUND('',#4011,.T.) ;
#808 = FACE_BOUND('',#4012,.T.) ;
#809 = FACE_BOUND('',#4013,.T.) ;
#810 = FACE_BOUND('',#4014,.T.) ;
#811 = FACE_BOUND('',#4016,.T.) ;
#812 = FACE_BOUND('',#4017,.T.) ;
#813 = FACE_BOUND('',#4018,.T.) ;
#814 = FACE_BOUND('',#4019,.T.) ;
#815 = FACE_BOUND('',#4020,.T.) ;
#816 = FACE_BOUND('',#4021,.T.) ;
#817 = FACE_BOUND('',#4022,.T.) ;
#818 = FACE_BOUND('',#4023,.T.) ;
#819 = FACE_BOUND('',#4024,.T.) ;
#820 = FACE_BOUND('',#4025,.T.) ;
#821 = FACE_BOUND('',#4026,.T.) ;
#822 = FACE_BOUND('',#4027,.T.) ;
#823 = FACE_BOUND('',#4028,.T.) ;
#824 = FACE_BOUND('',#4029,.T.) ;
#825 = FACE_BOUND('',#4030,.T.) ;
#826 = FACE_BOUND('',#4031,.T.) ;
#827 = FACE_BOUND('',#4032,.T.) ;
#828 = FACE_BOUND('',#4033,.T.) ;
#829 = FACE_BOUND('',#4034,.T.) ;
#830 = FACE_BOUND('',#4035,.T.) ;
#831 = FACE_BOUND('',#4036,.T.) ;
#832 = FACE_BOUND('',#4037,.T.) ;
#833 = FACE_BOUND('',#4038,.T.) ;
#834 = FACE_BOUND('',#4039,.T.) ;
#835 = FACE_BOUND('',#4040,.T.) ;
#836 = FACE_BOUND('',#4041,.T.) ;
#837 = FACE_BOUND('',#4042,.T.) ;
#838 = FACE_BOUND('',#4043,.T.) ;
#839 = FACE_BOUND('',#4045,.T.) ;
#840 = FACE_BOUND('',#4047,.T.) ;
#841 = FACE_BOUND('',#4051,.T.) ;
#842 = FACE_BOUND('',#4054,.T.) ;
#843 = FACE_BOUND('',#4057,.T.) ;
#844 = FACE_BOUND('',#4059,.T.) ;
#845 = FACE_BOUND('',#4063,.T.) ;
#846 = FACE_BOUND('',#4066,.T.) ;
#847 = FACE_BOUND('',#4071,.T.) ;
#848 = FACE_BOUND('',#4073,.T.) ;
#849 = FACE_BOUND('',#4084,.T.) ;
#850 = FACE_BOUND('',#4092,.T.) ;
#851 = FACE_BOUND('',#4138,.T.) ;
#852 = FACE_BOUND('',#4148,.T.) ;
#853 = FACE_BOUND('',#4150,.T.) ;
#854 = FACE_BOUND('',#4171,.T.) ;
#855 = FACE_BOUND('',#4175,.T.) ;
#856 = FACE_BOUND('',#4176,.T.) ;
#857 = FACE_BOUND('',#4291,.T.) ;
#858 = FACE_BOUND('',#4298,.T.) ;
#859 = FACE_BOUND('',#4301,.T.) ;
#860 = FACE_BOUND('',#4315,.T.) ;
#861 = FACE_BOUND('',#4329,.T.) ;
#862 = FACE_BOUND('',#4348,.T.) ;
#863 = FACE_BOUND('',#4382,.T.) ;
#864 = FACE_BOUND('',#4383,.T.) ;
#865 = FACE_BOUND('',#4386,.T.) ;
#866 = FACE_BOUND('',#4387,.T.) ;
#867 = FACE_BOUND('',#4390,.T.) ;
#868 = FACE_BOUND('',#4391,.T.) ;
#869 = FACE_BOUND('',#4394,.T.) ;
#870 = FACE_BOUND('',#4395,.T.) ;
#871 = FACE_BOUND('',#4402,.T.) ;
#872 = FACE_BOUND('',#4404,.T.) ;
#873 = FACE_BOUND('',#4417,.T.) ;
#874 = FACE_BOUND('',#4423,.T.) ;
#875 = FACE_BOUND('',#4425,.T.) ;
#876 = FACE_BOUND('',#4451,.T.) ;
#877 = FACE_BOUND('',#4452,.T.) ;
#878 = FACE_BOUND('',#4454,.T.) ;
#879 = FACE_BOUND('',#4456,.T.) ;
#880 = FACE_BOUND('',#4460,.T.) ;
#881 = FACE_BOUND('',#4462,.T.) ;
#882 = FACE_BOUND('',#4464,.T.) ;
#883 = FACE_BOUND('',#4467,.T.) ;
#884 = FACE_BOUND('',#4472,.T.) ;
#885 = FACE_BOUND('',#4488,.T.) ;
#886 = FACE_BOUND('',#4496,.T.) ;
#887 = FACE_BOUND('',#4498,.T.) ;
#888 = FACE_BOUND('',#4502,.T.) ;
#889 = FACE_BOUND('',#4554,.T.) ;
#890 = FACE_BOUND('',#4555,.T.) ;
#891 = FACE_BOUND('',#4556,.T.) ;
#892 = FACE_BOUND('',#4557,.T.) ;
#893 = FACE_BOUND('',#4558,.T.) ;
#894 = FACE_BOUND('',#4559,.T.) ;
#895 = FACE_BOUND('',#4560,.T.) ;
#896 = FACE_BOUND('',#4561,.T.) ;
#897 = FACE_BOUND('',#4562,.T.) ;
#898 = FACE_BOUND('',#4564,.T.) ;
#899 = FACE_BOUND('',#4566,.T.) ;
#900 = FACE_BOUND('',#4570,.T.) ;
#901 = FACE_BOUND('',#4572,.T.) ;
#902 = FACE_BOUND('',#4577,.T.) ;
#903 = FACE_BOUND('',#4590,.T.) ;
#904 = FACE_BOUND('',#4596,.T.) ;
#905 = FACE_BOUND('',#4600,.T.) ;
#906 = FACE_BOUND('',#4608,.T.) ;
#907 = FACE_BOUND('',#4610,.T.) ;
#908 = FACE_BOUND('',#4615,.T.) ;
#909 = FACE_BOUND('',#4617,.T.) ;
#910 = FACE_BOUND('',#4625,.T.) ;
#911 = FACE_BOUND('',#4629,.T.) ;
#912 = FACE_BOUND('',#4633,.T.) ;
#913 = FACE_BOUND('',#4635,.T.) ;
#914 = FACE_BOUND('',#4643,.T.) ;
#915 = FACE_BOUND('',#4644,.T.) ;
#916 = FACE_BOUND('',#4645,.T.) ;
#917 = FACE_BOUND('',#4646,.T.) ;
#918 = FACE_BOUND('',#4647,.T.) ;
#919 = FACE_BOUND('',#4649,.T.) ;
#920 = FACE_BOUND('',#4650,.T.) ;
#921 = FACE_BOUND('',#4651,.T.) ;
#922 = FACE_BOUND('',#4652,.T.) ;
#923 = FACE_BOUND('',#4653,.T.) ;
#924 = FACE_BOUND('',#4661,.T.) ;
#925 = FACE_BOUND('',#4662,.T.) ;
#926 = FACE_BOUND('',#4663,.T.) ;
#927 = FACE_BOUND('',#4664,.T.) ;
#928 = FACE_BOUND('',#4665,.T.) ;
#929 = FACE_BOUND('',#4667,.T.) ;
#930 = FACE_BOUND('',#4668,.T.) ;
#931 = FACE_BOUND('',#4669,.T.) ;
#932 = FACE_BOUND('',#4670,.T.) ;
#933 = FACE_BOUND('',#4671,.T.) ;
#934 = FACE_BOUND('',#4679,.T.) ;
#935 = FACE_BOUND('',#4681,.T.) ;
#936 = FACE_BOUND('',#4683,.T.) ;
#937 = FACE_BOUND('',#4684,.T.) ;
#938 = FACE_BOUND('',#4688,.T.) ;
#939 = FACE_BOUND('',#4690,.T.) ;
#940 = FACE_BOUND('',#4691,.T.) ;
#941 = FACE_BOUND('',#4694,.T.) ;
#942 = FACE_BOUND('',#4700,.T.) ;
#943 = FACE_BOUND('',#4704,.T.) ;
#944 = FACE_BOUND('',#4706,.T.) ;
#945 = FACE_BOUND('',#4711,.T.) ;
#946 = FACE_BOUND('',#4717,.T.) ;
#947 = FACE_BOUND('',#4728,.T.) ;
#948 = FACE_BOUND('',#4739,.T.) ;
#949 = FACE_BOUND('',#4744,.T.) ;
#950 = FACE_BOUND('',#4750,.T.) ;
#951 = B_SPLINE_CURVE_WITH_KNOTS('',3,(#19746,#19747,#19748,#19749,#19750,
#19751,#19752,#19753,#19754,#19755,#19756,#19757,#19758,#19759,#19760,#19761),
 .UNSPECIFIED.,.F.,.F.,(4,2,2,2,2,2,2,4),(0.687250434098959,0.82687421960189,
1.25301704446935,1.67915986933681,2.11450443098489,2.54984899263297,2.96432241698031,
3.37879584132764),.UNSPECIFIED.) ;
#952 = B_SPLINE_CURVE_WITH_KNOTS('',3,(#19763,#19764,#19765,#19766,#19767,
#19768,#19769,#19770,#19771,#19772,#19773,#19774,#19775,#19776,#19777,#19778),
 .UNSPECIFIED.,.F.,.F.,(4,2,2,2,2,2,2,4),(3.37879584132764,3.79326926567498,
4.20774269002231,4.6430872516704,5.07843181331848,5.50457463818594,5.9307174630534,
6.07034124855633),.UNSPECIFIED.) ;
#953 = B_SPLINE_CURVE_WITH_KNOTS('',3,(#19782,#19783,#19784,#19785,#19786,
#19787,#19788,#19789,#19790,#19791,#19792,#19793,#19794,#19795,#19796,#19797,
#19798,#19799,#19800,#19801,#19802,#19803,#19804),.UNSPECIFIED.,.F.,.F.,
(4,2,2,2,2,3,2,2,2,2,4),(-1.37470917955979,-1.12781391794867,-0.8458604384615,
-0.563906958974332,-0.281953479487166,0.,0.281953479487167,0.563906958974333,
0.8458604384615,1.12781391794867,1.37470917955955),.UNSPECIFIED.) ;
#954 = B_SPLINE_CURVE_WITH_KNOTS('',3,(#19913,#19914,#19915,#19916,#19917,
#19918,#19919,#19920,#19921,#19922,#19923,#19924,#19925,#19926,#19927,#19928,
#19929,#19930,#19931,#19932,#19933,#19934,#19935,#19936,#19937,#19938),
 .UNSPECIFIED.,.F.,.F.,(4,2,2,2,2,2,2,2,2,2,2,2,4),(0.,0.56410198036302,
0.84615297054453,1.12820396072604,1.41660602376442,1.7050080868028,1.99341014984119,
2.28181221287957,2.87260145541368,3.46339069794779,4.02908355018852,4.31192997630889,
4.59477640242925),.UNSPECIFIED.) ;
#955 = B_SPLINE_CURVE_WITH_KNOTS('',3,(#19939,#19940,#19941,#19942,#19943,
#19944,#19945,#19946,#19947,#19948,#19949,#19950,#19951,#19952,#19953,#19954,
#19955,#19956,#19957,#19958,#19959,#19960,#19961,#19962,#19963,#19964),
 .UNSPECIFIED.,.F.,.F.,(4,2,2,2,2,2,2,2,2,2,2,2,4),(4.59477640242925,4.87762282854962,
5.16046925466999,5.72616210691072,6.31695134944483,6.90774059197894,7.19614265501732,
7.4845447180557,7.77294678109409,8.06134884413247,8.34339983431398,8.62545082449549,
9.18955280485851),.UNSPECIFIED.) ;
#956 = B_SPLINE_CURVE_WITH_KNOTS('',3,(#21637,#21638,#21639,#21640,#21641,
#21642,#21643,#21644,#21645,#21646,#21647,#21648,#21649,#21650),
 .UNSPECIFIED.,.F.,.F.,(4,2,2,2,2,2,4),(1.10605212017019,1.19682866015767,
1.42236457431749,1.64790048847731,1.87343640263713,2.09897231679695,2.18974885678443),
 .UNSPECIFIED.) ;
#957 = B_SPLINE_CURVE_WITH_KNOTS('',3,(#21663,#21664,#21665,#21666,#21667,
#21668,#21669,#21670,#21671,#21672,#21673,#21674,#21675,#21676,#21677,#21678,
#21679,#21680,#21681,#21682,#21683,#21684,#21685,#21686,#21687,#21688),
 .UNSPECIFIED.,.F.,.F.,(4,2,2,2,2,2,2,2,2,2,2,2,4),(1.20535125846133,1.58564147586808,
1.96593169327483,2.13946869190595,2.31300569053706,2.5849459608724,2.85688623120774,
3.12882650154308,3.40076677187842,3.57430377050953,3.74784076914065,4.1281309865474,
4.50842120395415),.UNSPECIFIED.) ;
#958 = B_SPLINE_CURVE_WITH_KNOTS('',3,(#21860,#21861,#21862,#21863,#21864,
#21865,#21866,#21867,#21868,#21869),.UNSPECIFIED.,.F.,.F.,(4,2,2,2,4),(2.19179053945309,
2.41386787047132,2.73532606912548,3.05678426777964,3.27886159879787),
 .UNSPECIFIED.) ;
#959 = B_SPLINE_CURVE_WITH_KNOTS('',3,(#21899,#21900,#21901,#21902,#21903,
#21904,#21905,#21906,#21907,#21908,#21909,#21910,#21911,#21912,#21913,#21914,
#21915,#21916,#21917,#21918,#21919,#21920),.UNSPECIFIED.,.F.,.F.,(4,2,2,
2,2,2,2,2,2,2,4),(1.21055307378235,1.62541412185573,2.04027516992911,2.46215750524915,
2.67309867290916,2.88403984056918,3.0949810082292,3.30592217588921,3.72780451120925,
4.14266555928263,4.557526607356),.UNSPECIFIED.) ;
#960 = B_SPLINE_CURVE_WITH_KNOTS('',3,(#21996,#21997,#21998,#21999,#22000,
#22001),.UNSPECIFIED.,.F.,.F.,(4,2,4),(3.13976161696689,3.31479971489035,
3.53911083723209),.UNSPECIFIED.) ;
#961 = B_SPLINE_CURVE_WITH_KNOTS('',3,(#22002,#22003,#22004,#22005,#22006,
#22007,#22008,#22009,#22010,#22011,#22012,#22013,#22014,#22015,#22016,#22017,
#22018,#22019,#22020,#22021,#22022,#22023,#22024,#22025),.UNSPECIFIED.,
 .F.,.F.,(4,2,2,2,2,2,2,2,2,2,2,4),(0.,0.224311122341738,0.448622244683475,
0.897244489366951,1.3333999539915,1.55147768630377,1.76955541861604,1.98763315092831,
2.20571088324059,2.64186634786513,3.09048859254861,3.13976161696689),
 .UNSPECIFIED.) ;
#962 = B_SPLINE_CURVE_WITH_KNOTS('',3,(#22053,#22054,#22055,#22056,#22057,
#22058,#22059,#22060,#22061,#22062,#22063,#22064,#22065,#22066),
 .UNSPECIFIED.,.F.,.F.,(4,2,2,2,2,2,4),(-3.53911083723208,-3.31479971489035,
-3.09048859254861,-2.64186634786513,-2.20571088324059,-1.98763315092831,
-1.87498686215861),.UNSPECIFIED.) ;
#963 = B_SPLINE_CURVE_WITH_KNOTS('',3,(#22068,#22069,#22070,#22071,#22072,
#22073,#22074,#22075,#22076,#22077,#22078,#22079,#22080,#22081,#22082,#22083),
 .UNSPECIFIED.,.F.,.F.,(4,2,2,2,2,2,2,4),(-1.87498686215861,-1.76955541861604,
-1.55147768630377,-1.3333999539915,-0.89724448936695,-0.448622244683476,
-0.224311122341738,0.),.UNSPECIFIED.) ;
#964 = B_SPLINE_CURVE_WITH_KNOTS('',3,(#22406,#22407,#22408,#22409,#22410,
#22411),.UNSPECIFIED.,.F.,.F.,(4,2,4),(0.306797486954004,6.07243999004955,
11.9854458646039),.UNSPECIFIED.) ;
#965 = B_SPLINE_CURVE_WITH_KNOTS('',3,(#22413,#22414,#22415,#22416,#22417,
#22418,#22419,#22420,#22421,#22422,#22423,#22424,#22425,#22426,#22427,#22428),
 .UNSPECIFIED.,.F.,.F.,(4,3,3,3,3,4),(-22.7491660875703,-22.7326322777483,
-11.3663161388741,-8.43127796455208,-7.52321841795695,-0.0683548158626444),
 .UNSPECIFIED.) ;
#966 = B_SPLINE_CURVE_WITH_KNOTS('',3,(#22430,#22431,#22432,#22433,#22434,
#22435,#22436),.UNSPECIFIED.,.F.,.F.,(4,3,4),(0.149401224909902,0.242876764795977,
0.248953560391612),.UNSPECIFIED.) ;
#967 = B_SPLINE_CURVE_WITH_KNOTS('',3,(#22438,#22439,#22440,#22441,#22442,
#22443,#22444,#22445,#22446,#22447),.UNSPECIFIED.,.F.,.F.,(4,2,2,2,4),(0.0182113449411267,
0.579498375271715,1.16103870949885,1.68899220567266,2.20049000979166),
 .UNSPECIFIED.) ;
#968 = B_SPLINE_CURVE_WITH_KNOTS('',3,(#22449,#22450,#22451,#22452,#22453,
#22454,#22455),.UNSPECIFIED.,.F.,.F.,(4,3,4),(-0.00607546474194351,0.,0.0934550397936403),
 .UNSPECIFIED.) ;
#969 = B_SPLINE_CURVE_WITH_KNOTS('',3,(#22456,#22457,#22458,#22459,#22460,
#22461,#22462,#22463,#22464,#22465,#22466,#22467,#22468,#22469,#22470,#22471,
#22472,#22473,#22474),.UNSPECIFIED.,.F.,.F.,(4,3,3,3,3,3,4),(-8.32916619482315,
-6.19701983076071,-5.68275153370131,-5.33626613109357,-0.491091685615563,
0.,0.00607621245833095),.UNSPECIFIED.) ;
#970 = B_SPLINE_CURVE_WITH_KNOTS('',3,(#22525,#22526,#22527,#22528,#22529,
#22530),.UNSPECIFIED.,.F.,.F.,(4,2,4),(0.330130434724689,7.1450073655251,
14.1316592404919),.UNSPECIFIED.) ;
#971 = B_SPLINE_CURVE_WITH_KNOTS('',3,(#22532,#22533,#22534,#22535,#22536,
#22537,#22538,#22539,#22540,#22541,#22542,#22543,#22544,#22545,#22546,#22547),
 .UNSPECIFIED.,.F.,.F.,(4,3,3,3,3,4),(-0.00607619681590831,0.,4.17713740634383,
5.25576768694509,5.58948106622994,8.32915431888067),.UNSPECIFIED.) ;
#972 = B_SPLINE_CURVE_WITH_KNOTS('',3,(#22549,#22550,#22551,#22552,#22553,
#22554,#22555),.UNSPECIFIED.,.F.,.F.,(4,3,4),(-0.093455064791989,0.,0.00607547210165982),
 .UNSPECIFIED.) ;
#973 = B_SPLINE_CURVE_WITH_KNOTS('',3,(#22556,#22557,#22558,#22559,#22560,
#22561,#22562,#22563,#22564,#22565,#22566,#22567),.UNSPECIFIED.,.F.,.F.,
(4,2,2,2,2,4),(0.0230676064321383,0.582322749083777,1.16480388155931,1.75243736265584,
2.22755255780229,2.68204291945575),.UNSPECIFIED.) ;
#974 = B_SPLINE_CURVE_WITH_KNOTS('',3,(#22605,#22606,#22607,#22608,#22609,
#22610),.UNSPECIFIED.,.F.,.F.,(4,2,4),(0.306797486954258,6.07243999011767,
11.9854458647428),.UNSPECIFIED.) ;
#975 = B_SPLINE_CURVE_WITH_KNOTS('',3,(#22612,#22613,#22614,#22615,#22616,
#22617,#22618,#22619,#22620,#22621,#22622,#22623,#22624,#22625,#22626,#22627),
 .UNSPECIFIED.,.F.,.F.,(4,3,3,3,3,4),(-22.7491696598115,-22.732635833168,
-11.366317916584,-8.43127594084112,-7.52321777514952,-0.0683548158626444),
 .UNSPECIFIED.) ;
#976 = B_SPLINE_CURVE_WITH_KNOTS('',3,(#22629,#22630,#22631,#22632,#22633,
#22634,#22635),.UNSPECIFIED.,.F.,.F.,(4,3,4),(0.149401210175699,0.242876791624169,
0.248953579588731),.UNSPECIFIED.) ;
#977 = B_SPLINE_CURVE_WITH_KNOTS('',3,(#22636,#22637,#22638,#22639,#22640,
#22641,#22642,#22643,#22644,#22645),.UNSPECIFIED.,.F.,.F.,(4,2,2,2,4),(0.0182113449411156,
0.579498375271719,1.16103870949884,1.68899220567264,2.20049000979168),
 .UNSPECIFIED.) ;
#978 = B_SPLINE_CURVE_WITH_KNOTS('',3,(#22695,#22696,#22697,#22698,#22699,
#22700),.UNSPECIFIED.,.F.,.F.,(4,2,4),(0.330130434724726,7.14500736553715,
14.1316592405166),.UNSPECIFIED.) ;
#979 = B_SPLINE_CURVE_WITH_KNOTS('',3,(#22701,#22702,#22703,#22704,#22705,
#22706,#22707,#22708,#22709,#22710,#22711,#22712),.UNSPECIFIED.,.F.,.F.,
(4,2,2,2,2,4),(0.0230676064320783,0.582322749083774,1.1648038815593,1.75243736265581,
2.22755255780225,2.68204291945565),.UNSPECIFIED.) ;
#980 = B_SPLINE_CURVE_WITH_KNOTS('',3,(#23034,#23035,#23036,#23037,#23038,
#23039,#23040,#23041,#23042,#23043,#23044,#23045,#23046,#23047,#23048,#23049,
#23050,#23051,#23052,#23053,#23054,#23055,#23056,#23057,#23058,#23059),
 .UNSPECIFIED.,.F.,.F.,(4,2,2,2,2,2,2,2,2,2,2,2,4),(0.,0.268031600880283,
0.536063201760566,1.07212640352113,1.58977454134265,1.84859861025342,2.10742267916418,
2.36624674807494,2.6250708169857,3.14271895480722,3.67878215656779,3.94681375744807,
4.21484535832835),.UNSPECIFIED.) ;
#981 = B_SPLINE_CURVE_WITH_KNOTS('',3,(#23060,#23061,#23062,#23063,#23064,
#23065,#23066,#23067,#23068,#23069,#23070,#23071,#23072,#23073,#23074,#23075,
#23076,#23077,#23078,#23079,#23080,#23081,#23082,#23083,#23084,#23085),
 .UNSPECIFIED.,.F.,.F.,(4,2,2,2,2,2,2,2,2,2,2,2,4),(4.21484535832835,4.48287695920864,
4.75090856008892,5.28697176184949,5.80461989967101,6.06344396858177,6.32226803749253,
6.58109210640329,6.83991617531405,7.35756431313557,7.89362751489614,8.16165911577642,
8.42969071665671),.UNSPECIFIED.) ;
#982 = B_SPLINE_CURVE_WITH_KNOTS('',3,(#23105,#23106,#23107,#23108,#23109,
#23110,#23111,#23112,#23113,#23114,#23115,#23116,#23117,#23118,#23119,#23120,
#23121,#23122),.UNSPECIFIED.,.F.,.F.,(4,2,2,2,2,2,2,2,4),(6.84192042814915,
7.05142392525706,7.37435159053249,7.69727925580792,8.02020692108334,8.34313458635877,
8.6660622516342,8.98898991690963,9.19849341401755),.UNSPECIFIED.) ;
#983 = B_SPLINE_CURVE_WITH_KNOTS('',3,(#23124,#23125,#23126,#23127,#23128,
#23129,#23130,#23131,#23132,#23133,#23134,#23135,#23136,#23137,#23138,#23139,
#23140,#23141),.UNSPECIFIED.,.F.,.F.,(4,2,2,2,2,2,2,2,4),(1.49511581409358,
1.7046193112015,2.02754697647693,2.35047464175235,2.67340230702778,2.99632997230321,
3.31925763757864,3.64218530285406,3.85168879996198),.UNSPECIFIED.) ;
#984 = B_SPLINE_CURVE_WITH_KNOTS('',3,(#23620,#23621,#23622,#23623,#23624,
#23625,#23626,#23627,#23628,#23629,#23630,#23631,#23632,#23633,#23634,#23635,
#23636,#23637,#23638,#23639,#23640,#23641,#23642,#23643,#23644,#23645,#23646,
#23647,#23648,#23649),.UNSPECIFIED.,.F.,.F.,(4,2,2,2,2,2,2,2,2,2,2,2,2,
2,4),(-4.08940558183937,-3.82598745493601,-3.56256932803264,-3.29915120112928,
-3.03573307422591,-2.5402179325728,-2.29246036174624,-2.04470279091969,
-1.79694522009313,-1.54918764926658,-1.05367250761347,-0.7902543807101,
-0.526836253806733,-0.263418126903367,0.),.UNSPECIFIED.) ;
#985 = B_SPLINE_CURVE_WITH_KNOTS('',3,(#23796,#23797,#23798,#23799,#23800,
#23801,#23802,#23803,#23804,#23805,#23806,#23807,#23808,#23809),
 .UNSPECIFIED.,.F.,.F.,(4,2,2,2,2,2,4),(0.,0.222195827909919,0.444391655819838,
0.888783311639677,1.32318070684216,1.54037940444341,1.75757810204465),
 .UNSPECIFIED.) ;
#986 = B_SPLINE_CURVE_WITH_KNOTS('',3,(#23811,#23812,#23813,#23814,#23815,
#23816,#23817,#23818,#23819,#23820,#23821,#23822,#23823,#23824),
 .UNSPECIFIED.,.F.,.F.,(4,2,2,2,2,2,4),(5.27273430613395,5.48993300373519,
5.70713170133643,6.14152909653892,6.58592075235876,6.80811658026868,7.0303124081786),
 .UNSPECIFIED.) ;
#987 = B_SPLINE_CURVE_WITH_KNOTS('',3,(#23828,#23829,#23830,#23831,#23832,
#23833,#23834,#23835,#23836,#23837,#23838,#23839,#23840,#23841),
 .UNSPECIFIED.,.F.,.F.,(4,2,2,2,2,2,4),(0.,0.215433509152083,0.430867018304165,
0.86173403660833,1.28909704518263,1.50277854946978,1.71646005375693),
 .UNSPECIFIED.) ;
#988 = B_SPLINE_CURVE_WITH_KNOTS('',3,(#23843,#23844,#23845,#23846,#23847,
#23848,#23849,#23850,#23851,#23852,#23853,#23854,#23855,#23856),
 .UNSPECIFIED.,.F.,.F.,(4,2,2,2,2,2,4),(5.14938016127078,5.36306166555793,
5.57674316984508,6.00410617841938,6.43497319672355,6.65040670587563,6.86584021502771),
 .UNSPECIFIED.) ;
#989 = B_SPLINE_CURVE_WITH_KNOTS('',3,(#23857,#23858,#23859,#23860,#23861,
#23862,#23863,#23864,#23865,#23866,#23867,#23868,#23869,#23870,#23871,#23872,
#23873,#23874,#23875,#23876,#23877,#23878,#23879,#23880,#23881,#23882),
 .UNSPECIFIED.,.F.,.F.,(4,2,2,2,2,2,2,2,2,2,2,2,4),(1.71646005375693,1.93014155804408,
2.14382306233123,2.57118607090553,3.00205308920969,3.21748659836177,3.43292010751385,
3.64835361666594,3.86378712581802,4.29465414412218,4.72201715269648,4.93569865698363,
5.14938016127078),.UNSPECIFIED.) ;
#990 = B_SPLINE_CURVE_WITH_KNOTS('',3,(#23883,#23884,#23885,#23886,#23887,
#23888,#23889,#23890,#23891,#23892,#23893,#23894,#23895,#23896,#23897,#23898,
#23899,#23900,#23901,#23902,#23903,#23904,#23905,#23906,#23907,#23908),
 .UNSPECIFIED.,.F.,.F.,(4,2,2,2,2,2,2,2,2,2,2,2,4),(1.75757810204465,1.97477679964589,
2.19197549724714,2.62637289244962,3.07076454826946,3.29296037617938,3.5151562040893,
3.73735203199922,3.95954785990914,4.40393951572897,4.83833691093146,5.0555356085327,
5.27273430613395),.UNSPECIFIED.) ;
#991 = B_SPLINE_CURVE_WITH_KNOTS('',3,(#23937,#23938,#23939,#23940,#23941,
#23942,#23943,#23944,#23945,#23946,#23947,#23948,#23949),.UNSPECIFIED.,
 .F.,.F.,(4,3,2,2,2,4),(-0.0993179449412329,0.,0.274566149486996,0.549132298973992,
0.821321935999811,1.09351157302563),.UNSPECIFIED.) ;
#992 = B_SPLINE_CURVE_WITH_KNOTS('',3,(#23951,#23952,#23953,#23954,#23955,
#23956,#23957,#23958,#23959,#23960,#23961,#23962,#23963,#23964,#23965,#23966,
#23967),.UNSPECIFIED.,.F.,.F.,(4,2,2,2,2,2,3,4),(-1.69011593432845,-1.48746936798106,
-1.28482280163367,-0.87952966893888,-0.43976483446944,-0.219882417234721,
0.,0.10342060321835),.UNSPECIFIED.) ;
#993 = B_SPLINE_CURVE_WITH_KNOTS('',3,(#23969,#23970,#23971,#23972,#23973,
#23974,#23975,#23976,#23977,#23978,#23979,#23980,#23981,#23982,#23983,#23984),
 .UNSPECIFIED.,.F.,.F.,(4,2,2,2,2,2,2,4),(-3.48365246791255,-3.38023186865691,
-3.16034945142219,-2.94046703418747,-2.50070219971803,-2.09540906702324,
-1.89276250067585,-1.69011593432845),.UNSPECIFIED.) ;
#994 = B_SPLINE_CURVE_WITH_KNOTS('',3,(#23987,#23988,#23989,#23990,#23991,
#23992,#23993,#23994,#23995,#23996,#23997,#23998),.UNSPECIFIED.,.F.,.F.,
(4,2,2,2,2,4),(1.09351157302563,1.36570121005145,1.63789084707727,1.91245699656426,
2.18702314605126,2.28634110246251),.UNSPECIFIED.) ;
#995 = B_SPLINE_CURVE_WITH_KNOTS('',3,(#24002,#24003,#24004,#24005,#24006,
#24007,#24008,#24009,#24010,#24011,#24012,#24013),.UNSPECIFIED.,.F.,.F.,
(4,2,2,2,2,4),(-2.28634109099249,-2.18702314605126,-1.91245699656426,-1.63789084707727,
-1.36570121005145,-1.09351157302563),.UNSPECIFIED.) ;
#996 = B_SPLINE_CURVE_WITH_KNOTS('',3,(#24017,#24018,#24019,#24020,#24021,
#24022,#24023,#24024,#24025,#24026,#24027,#24028,#24029,#24030,#24031,#24032),
 .UNSPECIFIED.,.F.,.F.,(4,2,2,2,2,2,2,4),(1.69011593432845,1.89276250067585,
2.09540906702324,2.50070219971803,2.94046703418747,3.16034945142219,3.38023186865691,
3.48365247187527),.UNSPECIFIED.) ;
#997 = B_SPLINE_CURVE_WITH_KNOTS('',3,(#24033,#24034,#24035,#24036,#24037,
#24038,#24039,#24040,#24041,#24042,#24043,#24044,#24045,#24046,#24047,#24048,
#24049),.UNSPECIFIED.,.F.,.F.,(4,3,2,2,2,2,2,4),(-0.103420599255634,0.,
0.21988241723472,0.43976483446944,0.87952966893888,1.28482280163367,1.48746936798106,
1.69011593432845),.UNSPECIFIED.) ;
#998 = B_SPLINE_CURVE_WITH_KNOTS('',3,(#24050,#24051,#24052,#24053,#24054,
#24055,#24056,#24057,#24058,#24059,#24060,#24061,#24062),.UNSPECIFIED.,
 .F.,.F.,(4,2,2,2,3,4),(-1.09351157302563,-0.821321935999811,-0.549132298973992,
-0.274566149486996,0.,0.0993179564112534),.UNSPECIFIED.) ;
#999 = B_SPLINE_CURVE_WITH_KNOTS('',3,(#24196,#24197,#24198,#24199,#24200,
#24201,#24202,#24203,#24204,#24205,#24206,#24207,#24208,#24209,#24210,#24211,
#24212,#24213,#24214),.UNSPECIFIED.,.F.,.F.,(4,2,2,2,3,2,2,2,4),(-0.471793481292107,
-0.373843585675949,-0.243618913657373,-0.121809456828687,0.,0.121809456828687,
0.243618913657373,0.373843585675949,0.471793481292107),.UNSPECIFIED.) ;
#1000 = B_SPLINE_CURVE_WITH_KNOTS('',3,(#24227,#24228,#24229,#24230,#24231,
#24232,#24233,#24234,#24235,#24236,#24237,#24238,#24239,#24240,#24241,#24242,
#24243,#24244),.UNSPECIFIED.,.F.,.F.,(4,2,2,2,2,2,2,2,4),(0.554019722357309,
0.651969617973467,0.782194289992043,0.904003746820729,1.02581320364942,
1.1476226604781,1.26943211730679,1.39965678932537,1.49760668494152),
 .UNSPECIFIED.) ;
#1001 = LINE('',#19715,#1837) ;
#1002 = LINE('',#19717,#1838) ;
#1003 = LINE('',#19720,#1839) ;
#1004 = LINE('',#19725,#1840) ;
#1005 = LINE('',#19729,#1841) ;
#1006 = LINE('',#19733,#1842) ;
#1007 = LINE('',#19738,#1843) ;
#1008 = LINE('',#19742,#1844) ;
#1009 = LINE('',#19780,#1845) ;
#1010 = LINE('',#19805,#1846) ;
#1011 = LINE('',#19810,#1847) ;
#1012 = LINE('',#19825,#1848) ;
#1013 = LINE('',#19831,#1849) ;
#1014 = LINE('',#19837,#1850) ;
#1015 = LINE('',#19843,#1851) ;
#1016 = LINE('',#19849,#1852) ;
#1017 = LINE('',#19855,#1853) ;
#1018 = LINE('',#19860,#1854) ;
#1019 = LINE('',#19862,#1855) ;
#1020 = LINE('',#19864,#1856) ;
#1021 = LINE('',#19866,#1857) ;
#1022 = LINE('',#19868,#1858) ;
#1023 = LINE('',#19869,#1859) ;
#1024 = LINE('',#19872,#1860) ;
#1025 = LINE('',#19874,#1861) ;
#1026 = LINE('',#19875,#1862) ;
#1027 = LINE('',#19879,#1863) ;
#1028 = LINE('',#19883,#1864) ;
#1029 = LINE('',#19884,#1865) ;
#1030 = LINE('',#19885,#1866) ;
#1031 = LINE('',#19887,#1867) ;
#1032 = LINE('',#19891,#1868) ;
#1033 = LINE('',#19894,#1869) ;
#1034 = LINE('',#19895,#1870) ;
#1035 = LINE('',#19900,#1871) ;
#1036 = LINE('',#19905,#1872) ;
#1037 = LINE('',#19909,#1873) ;
#1038 = LINE('',#19968,#1874) ;
#1039 = LINE('',#19972,#1875) ;
#1040 = LINE('',#19983,#1876) ;
#1041 = LINE('',#19990,#1877) ;
#1042 = LINE('',#20001,#1878) ;
#1043 = LINE('',#20007,#1879) ;
#1044 = LINE('',#20014,#1880) ;
#1045 = LINE('',#20020,#1881) ;
#1046 = LINE('',#20024,#1882) ;
#1047 = LINE('',#20033,#1883) ;
#1048 = LINE('',#20039,#1884) ;
#1049 = LINE('',#20045,#1885) ;
#1050 = LINE('',#20051,#1886) ;
#1051 = LINE('',#20057,#1887) ;
#1052 = LINE('',#20063,#1888) ;
#1053 = LINE('',#20069,#1889) ;
#1054 = LINE('',#20075,#1890) ;
#1055 = LINE('',#20081,#1891) ;
#1056 = LINE('',#20088,#1892) ;
#1057 = LINE('',#20094,#1893) ;
#1058 = LINE('',#20101,#1894) ;
#1059 = LINE('',#20109,#1895) ;
#1060 = LINE('',#20114,#1896) ;
#1061 = LINE('',#20121,#1897) ;
#1062 = LINE('',#20130,#1898) ;
#1063 = LINE('',#20139,#1899) ;
#1064 = LINE('',#20145,#1900) ;
#1065 = LINE('',#20151,#1901) ;
#1066 = LINE('',#20157,#1902) ;
#1067 = LINE('',#20163,#1903) ;
#1068 = LINE('',#20169,#1904) ;
#1069 = LINE('',#20175,#1905) ;
#1070 = LINE('',#20181,#1906) ;
#1071 = LINE('',#20189,#1907) ;
#1072 = LINE('',#20191,#1908) ;
#1073 = LINE('',#20193,#1909) ;
#1074 = LINE('',#20194,#1910) ;
#1075 = LINE('',#20199,#1911) ;
#1076 = LINE('',#20200,#1912) ;
#1077 = LINE('',#20204,#1913) ;
#1078 = LINE('',#20205,#1914) ;
#1079 = LINE('',#20206,#1915) ;
#1080 = LINE('',#20208,#1916) ;
#1081 = LINE('',#20213,#1917) ;
#1082 = LINE('',#20220,#1918) ;
#1083 = LINE('',#20229,#1919) ;
#1084 = LINE('',#20234,#1920) ;
#1085 = LINE('',#20240,#1921) ;
#1086 = LINE('',#20246,#1922) ;
#1087 = LINE('',#20254,#1923) ;
#1088 = LINE('',#20259,#1924) ;
#1089 = LINE('',#20269,#1925) ;
#1090 = LINE('',#20276,#1926) ;
#1091 = LINE('',#20283,#1927) ;
#1092 = LINE('',#20290,#1928) ;
#1093 = LINE('',#20297,#1929) ;
#1094 = LINE('',#20304,#1930) ;
#1095 = LINE('',#20311,#1931) ;
#1096 = LINE('',#20318,#1932) ;
#1097 = LINE('',#20325,#1933) ;
#1098 = LINE('',#20332,#1934) ;
#1099 = LINE('',#20339,#1935) ;
#1100 = LINE('',#20346,#1936) ;
#1101 = LINE('',#20353,#1937) ;
#1102 = LINE('',#20360,#1938) ;
#1103 = LINE('',#20367,#1939) ;
#1104 = LINE('',#20374,#1940) ;
#1105 = LINE('',#20381,#1941) ;
#1106 = LINE('',#20388,#1942) ;
#1107 = LINE('',#20395,#1943) ;
#1108 = LINE('',#20402,#1944) ;
#1109 = LINE('',#20409,#1945) ;
#1110 = LINE('',#20416,#1946) ;
#1111 = LINE('',#20423,#1947) ;
#1112 = LINE('',#20430,#1948) ;
#1113 = LINE('',#20437,#1949) ;
#1114 = LINE('',#20443,#1950) ;
#1115 = LINE('',#20449,#1951) ;
#1116 = LINE('',#20455,#1952) ;
#1117 = LINE('',#20461,#1953) ;
#1118 = LINE('',#20467,#1954) ;
#1119 = LINE('',#20473,#1955) ;
#1120 = LINE('',#20479,#1956) ;
#1121 = LINE('',#20485,#1957) ;
#1122 = LINE('',#20491,#1958) ;
#1123 = LINE('',#20497,#1959) ;
#1124 = LINE('',#20503,#1960) ;
#1125 = LINE('',#20509,#1961) ;
#1126 = LINE('',#20515,#1962) ;
#1127 = LINE('',#20521,#1963) ;
#1128 = LINE('',#20527,#1964) ;
#1129 = LINE('',#20533,#1965) ;
#1130 = LINE('',#20539,#1966) ;
#1131 = LINE('',#20545,#1967) ;
#1132 = LINE('',#20551,#1968) ;
#1133 = LINE('',#20557,#1969) ;
#1134 = LINE('',#20563,#1970) ;
#1135 = LINE('',#20569,#1971) ;
#1136 = LINE('',#20575,#1972) ;
#1137 = LINE('',#20581,#1973) ;
#1138 = LINE('',#20587,#1974) ;
#1139 = LINE('',#20593,#1975) ;
#1140 = LINE('',#20599,#1976) ;
#1141 = LINE('',#20605,#1977) ;
#1142 = LINE('',#20621,#1978) ;
#1143 = LINE('',#20623,#1979) ;
#1144 = LINE('',#20632,#1980) ;
#1145 = LINE('',#20637,#1981) ;
#1146 = LINE('',#20650,#1982) ;
#1147 = LINE('',#20652,#1983) ;
#1148 = LINE('',#20661,#1984) ;
#1149 = LINE('',#20666,#1985) ;
#1150 = LINE('',#20672,#1986) ;
#1151 = LINE('',#20678,#1987) ;
#1152 = LINE('',#20686,#1988) ;
#1153 = LINE('',#20688,#1989) ;
#1154 = LINE('',#20690,#1990) ;
#1155 = LINE('',#20691,#1991) ;
#1156 = LINE('',#20695,#1992) ;
#1157 = LINE('',#20697,#1993) ;
#1158 = LINE('',#20699,#1994) ;
#1159 = LINE('',#20700,#1995) ;
#1160 = LINE('',#20713,#1996) ;
#1161 = LINE('',#20715,#1997) ;
#1162 = LINE('',#20717,#1998) ;
#1163 = LINE('',#20718,#1999) ;
#1164 = LINE('',#20722,#2000) ;
#1165 = LINE('',#20724,#2001) ;
#1166 = LINE('',#20726,#2002) ;
#1167 = LINE('',#20727,#2003) ;
#1168 = LINE('',#20729,#2004) ;
#1169 = LINE('',#20730,#2005) ;
#1170 = LINE('',#20740,#2006) ;
#1171 = LINE('',#20742,#2007) ;
#1172 = LINE('',#20744,#2008) ;
#1173 = LINE('',#20745,#2009) ;
#1174 = LINE('',#20749,#2010) ;
#1175 = LINE('',#20751,#2011) ;
#1176 = LINE('',#20753,#2012) ;
#1177 = LINE('',#20754,#2013) ;
#1178 = LINE('',#20756,#2014) ;
#1179 = LINE('',#20757,#2015) ;
#1180 = LINE('',#20762,#2016) ;
#1181 = LINE('',#20768,#2017) ;
#1182 = LINE('',#20772,#2018) ;
#1183 = LINE('',#20774,#2019) ;
#1184 = LINE('',#20776,#2020) ;
#1185 = LINE('',#20780,#2021) ;
#1186 = LINE('',#20782,#2022) ;
#1187 = LINE('',#20784,#2023) ;
#1188 = LINE('',#20788,#2024) ;
#1189 = LINE('',#20790,#2025) ;
#1190 = LINE('',#20792,#2026) ;
#1191 = LINE('',#20796,#2027) ;
#1192 = LINE('',#20798,#2028) ;
#1193 = LINE('',#20800,#2029) ;
#1194 = LINE('',#20804,#2030) ;
#1195 = LINE('',#20806,#2031) ;
#1196 = LINE('',#20808,#2032) ;
#1197 = LINE('',#20812,#2033) ;
#1198 = LINE('',#20814,#2034) ;
#1199 = LINE('',#20816,#2035) ;
#1200 = LINE('',#20820,#2036) ;
#1201 = LINE('',#20822,#2037) ;
#1202 = LINE('',#20824,#2038) ;
#1203 = LINE('',#20828,#2039) ;
#1204 = LINE('',#20830,#2040) ;
#1205 = LINE('',#20832,#2041) ;
#1206 = LINE('',#20836,#2042) ;
#1207 = LINE('',#20838,#2043) ;
#1208 = LINE('',#20840,#2044) ;
#1209 = LINE('',#20844,#2045) ;
#1210 = LINE('',#20846,#2046) ;
#1211 = LINE('',#20848,#2047) ;
#1212 = LINE('',#20852,#2048) ;
#1213 = LINE('',#20854,#2049) ;
#1214 = LINE('',#20855,#2050) ;
#1215 = LINE('',#20858,#2051) ;
#1216 = LINE('',#20859,#2052) ;
#1217 = LINE('',#20862,#2053) ;
#1218 = LINE('',#20864,#2054) ;
#1219 = LINE('',#20865,#2055) ;
#1220 = LINE('',#20867,#2056) ;
#1221 = LINE('',#20871,#2057) ;
#1222 = LINE('',#20874,#2058) ;
#1223 = LINE('',#20876,#2059) ;
#1224 = LINE('',#20877,#2060) ;
#1225 = LINE('',#20880,#2061) ;
#1226 = LINE('',#20881,#2062) ;
#1227 = LINE('',#20883,#2063) ;
#1228 = LINE('',#20887,#2064) ;
#1229 = LINE('',#20890,#2065) ;
#1230 = LINE('',#20891,#2066) ;
#1231 = LINE('',#20894,#2067) ;
#1232 = LINE('',#20896,#2068) ;
#1233 = LINE('',#20897,#2069) ;
#1234 = LINE('',#20899,#2070) ;
#1235 = LINE('',#20903,#2071) ;
#1236 = LINE('',#20906,#2072) ;
#1237 = LINE('',#20908,#2073) ;
#1238 = LINE('',#20909,#2074) ;
#1239 = LINE('',#20912,#2075) ;
#1240 = LINE('',#20913,#2076) ;
#1241 = LINE('',#20915,#2077) ;
#1242 = LINE('',#20919,#2078) ;
#1243 = LINE('',#20922,#2079) ;
#1244 = LINE('',#20923,#2080) ;
#1245 = LINE('',#20926,#2081) ;
#1246 = LINE('',#20928,#2082) ;
#1247 = LINE('',#20929,#2083) ;
#1248 = LINE('',#20931,#2084) ;
#1249 = LINE('',#20935,#2085) ;
#1250 = LINE('',#20938,#2086) ;
#1251 = LINE('',#20940,#2087) ;
#1252 = LINE('',#20941,#2088) ;
#1253 = LINE('',#20944,#2089) ;
#1254 = LINE('',#20945,#2090) ;
#1255 = LINE('',#20947,#2091) ;
#1256 = LINE('',#20951,#2092) ;
#1257 = LINE('',#20954,#2093) ;
#1258 = LINE('',#20955,#2094) ;
#1259 = LINE('',#20958,#2095) ;
#1260 = LINE('',#20960,#2096) ;
#1261 = LINE('',#20961,#2097) ;
#1262 = LINE('',#20963,#2098) ;
#1263 = LINE('',#20967,#2099) ;
#1264 = LINE('',#20970,#2100) ;
#1265 = LINE('',#20972,#2101) ;
#1266 = LINE('',#20973,#2102) ;
#1267 = LINE('',#20976,#2103) ;
#1268 = LINE('',#20977,#2104) ;
#1269 = LINE('',#20979,#2105) ;
#1270 = LINE('',#20983,#2106) ;
#1271 = LINE('',#20986,#2107) ;
#1272 = LINE('',#20987,#2108) ;
#1273 = LINE('',#20990,#2109) ;
#1274 = LINE('',#20992,#2110) ;
#1275 = LINE('',#20993,#2111) ;
#1276 = LINE('',#20995,#2112) ;
#1277 = LINE('',#20999,#2113) ;
#1278 = LINE('',#21002,#2114) ;
#1279 = LINE('',#21004,#2115) ;
#1280 = LINE('',#21005,#2116) ;
#1281 = LINE('',#21008,#2117) ;
#1282 = LINE('',#21009,#2118) ;
#1283 = LINE('',#21011,#2119) ;
#1284 = LINE('',#21015,#2120) ;
#1285 = LINE('',#21018,#2121) ;
#1286 = LINE('',#21019,#2122) ;
#1287 = LINE('',#21022,#2123) ;
#1288 = LINE('',#21023,#2124) ;
#1289 = LINE('',#21025,#2125) ;
#1290 = LINE('',#21029,#2126) ;
#1291 = LINE('',#21035,#2127) ;
#1292 = LINE('',#21037,#2128) ;
#1293 = LINE('',#21039,#2129) ;
#1294 = LINE('',#21040,#2130) ;
#1295 = LINE('',#21044,#2131) ;
#1296 = LINE('',#21046,#2132) ;
#1297 = LINE('',#21048,#2133) ;
#1298 = LINE('',#21049,#2134) ;
#1299 = LINE('',#21051,#2135) ;
#1300 = LINE('',#21052,#2136) ;
#1301 = LINE('',#21054,#2137) ;
#1302 = LINE('',#21056,#2138) ;
#1303 = LINE('',#21063,#2139) ;
#1304 = LINE('',#21069,#2140) ;
#1305 = LINE('',#21077,#2141) ;
#1306 = LINE('',#21079,#2142) ;
#1307 = LINE('',#21081,#2143) ;
#1308 = LINE('',#21082,#2144) ;
#1309 = LINE('',#21085,#2145) ;
#1310 = LINE('',#21087,#2146) ;
#1311 = LINE('',#21088,#2147) ;
#1312 = LINE('',#21091,#2148) ;
#1313 = LINE('',#21092,#2149) ;
#1314 = LINE('',#21095,#2150) ;
#1315 = LINE('',#21096,#2151) ;
#1316 = LINE('',#21099,#2152) ;
#1317 = LINE('',#21101,#2153) ;
#1318 = LINE('',#21103,#2154) ;
#1319 = LINE('',#21105,#2155) ;
#1320 = LINE('',#21106,#2156) ;
#1321 = LINE('',#21109,#2157) ;
#1322 = LINE('',#21111,#2158) ;
#1323 = LINE('',#21112,#2159) ;
#1324 = LINE('',#21115,#2160) ;
#1325 = LINE('',#21117,#2161) ;
#1326 = LINE('',#21118,#2162) ;
#1327 = LINE('',#21120,#2163) ;
#1328 = LINE('',#21121,#2164) ;
#1329 = LINE('',#21129,#2165) ;
#1330 = LINE('',#21136,#2166) ;
#1331 = LINE('',#21141,#2167) ;
#1332 = LINE('',#21145,#2168) ;
#1333 = LINE('',#21150,#2169) ;
#1334 = LINE('',#21154,#2170) ;
#1335 = LINE('',#21159,#2171) ;
#1336 = LINE('',#21163,#2172) ;
#1337 = LINE('',#21167,#2173) ;
#1338 = LINE('',#21169,#2174) ;
#1339 = LINE('',#21170,#2175) ;
#1340 = LINE('',#21173,#2176) ;
#1341 = LINE('',#21175,#2177) ;
#1342 = LINE('',#21176,#2178) ;
#1343 = LINE('',#21179,#2179) ;
#1344 = LINE('',#21181,#2180) ;
#1345 = LINE('',#21182,#2181) ;
#1346 = LINE('',#21184,#2182) ;
#1347 = LINE('',#21186,#2183) ;
#1348 = LINE('',#21187,#2184) ;
#1349 = LINE('',#21188,#2185) ;
#1350 = LINE('',#21190,#2186) ;
#1351 = LINE('',#21193,#2187) ;
#1352 = LINE('',#21194,#2188) ;
#1353 = LINE('',#21196,#2189) ;
#1354 = LINE('',#21197,#2190) ;
#1355 = LINE('',#21205,#2191) ;
#1356 = LINE('',#21465,#2192) ;
#1357 = LINE('',#21473,#2193) ;
#1358 = LINE('',#21477,#2194) ;
#1359 = LINE('',#21480,#2195) ;
#1360 = LINE('',#21483,#2196) ;
#1361 = LINE('',#21486,#2197) ;
#1362 = LINE('',#21492,#2198) ;
#1363 = LINE('',#21499,#2199) ;
#1364 = LINE('',#21504,#2200) ;
#1365 = LINE('',#21511,#2201) ;
#1366 = LINE('',#21515,#2202) ;
#1367 = LINE('',#21518,#2203) ;
#1368 = LINE('',#21521,#2204) ;
#1369 = LINE('',#21524,#2205) ;
#1370 = LINE('',#21530,#2206) ;
#1371 = LINE('',#21537,#2207) ;
#1372 = LINE('',#21542,#2208) ;
#1373 = LINE('',#21549,#2209) ;
#1374 = LINE('',#21553,#2210) ;
#1375 = LINE('',#21556,#2211) ;
#1376 = LINE('',#21559,#2212) ;
#1377 = LINE('',#21562,#2213) ;
#1378 = LINE('',#21568,#2214) ;
#1379 = LINE('',#21575,#2215) ;
#1380 = LINE('',#21580,#2216) ;
#1381 = LINE('',#21587,#2217) ;
#1382 = LINE('',#21591,#2218) ;
#1383 = LINE('',#21594,#2219) ;
#1384 = LINE('',#21597,#2220) ;
#1385 = LINE('',#21600,#2221) ;
#1386 = LINE('',#21606,#2222) ;
#1387 = LINE('',#21613,#2223) ;
#1388 = LINE('',#21995,#2224) ;
#1389 = LINE('',#22030,#2225) ;
#1390 = LINE('',#22043,#2226) ;
#1391 = LINE('',#22088,#2227) ;
#1392 = LINE('',#22092,#2228) ;
#1393 = LINE('',#22096,#2229) ;
#1394 = LINE('',#22106,#2230) ;
#1395 = LINE('',#22116,#2231) ;
#1396 = LINE('',#22120,#2232) ;
#1397 = LINE('',#22124,#2233) ;
#1398 = LINE('',#22134,#2234) ;
#1399 = LINE('',#22144,#2235) ;
#1400 = LINE('',#22148,#2236) ;
#1401 = LINE('',#22152,#2237) ;
#1402 = LINE('',#22162,#2238) ;
#1403 = LINE('',#22172,#2239) ;
#1404 = LINE('',#22180,#2240) ;
#1405 = LINE('',#22194,#2241) ;
#1406 = LINE('',#22245,#2242) ;
#1407 = LINE('',#22248,#2243) ;
#1408 = LINE('',#22251,#2244) ;
#1409 = LINE('',#22253,#2245) ;
#1410 = LINE('',#22254,#2246) ;
#1411 = LINE('',#22260,#2247) ;
#1412 = LINE('',#22262,#2248) ;
#1413 = LINE('',#22263,#2249) ;
#1414 = LINE('',#22268,#2250) ;
#1415 = LINE('',#22275,#2251) ;
#1416 = LINE('',#22278,#2252) ;
#1417 = LINE('',#22281,#2253) ;
#1418 = LINE('',#22283,#2254) ;
#1419 = LINE('',#22284,#2255) ;
#1420 = LINE('',#22290,#2256) ;
#1421 = LINE('',#22292,#2257) ;
#1422 = LINE('',#22293,#2258) ;
#1423 = LINE('',#22298,#2259) ;
#1424 = LINE('',#22303,#2260) ;
#1425 = LINE('',#22305,#2261) ;
#1426 = LINE('',#22307,#2262) ;
#1427 = LINE('',#22308,#2263) ;
#1428 = LINE('',#22311,#2264) ;
#1429 = LINE('',#22313,#2265) ;
#1430 = LINE('',#22314,#2266) ;
#1431 = LINE('',#22317,#2267) ;
#1432 = LINE('',#22319,#2268) ;
#1433 = LINE('',#22320,#2269) ;
#1434 = LINE('',#22324,#2270) ;
#1435 = LINE('',#22325,#2271) ;
#1436 = LINE('',#22326,#2272) ;
#1437 = LINE('',#22329,#2273) ;
#1438 = LINE('',#22330,#2274) ;
#1439 = LINE('',#22333,#2275) ;
#1440 = LINE('',#22334,#2276) ;
#1441 = LINE('',#22336,#2277) ;
#1442 = LINE('',#22725,#2278) ;
#1443 = LINE('',#22727,#2279) ;
#1444 = LINE('',#22729,#2280) ;
#1445 = LINE('',#22730,#2281) ;
#1446 = LINE('',#22755,#2282) ;
#1447 = LINE('',#22756,#2283) ;
#1448 = LINE('',#22785,#2284) ;
#1449 = LINE('',#22810,#2285) ;
#1450 = LINE('',#22844,#2286) ;
#1451 = LINE('',#22850,#2287) ;
#1452 = LINE('',#22852,#2288) ;
#1453 = LINE('',#22854,#2289) ;
#1454 = LINE('',#22855,#2290) ;
#1455 = LINE('',#22858,#2291) ;
#1456 = LINE('',#22860,#2292) ;
#1457 = LINE('',#22861,#2293) ;
#1458 = LINE('',#22864,#2294) ;
#1459 = LINE('',#22865,#2295) ;
#1460 = LINE('',#22868,#2296) ;
#1461 = LINE('',#22869,#2297) ;
#1462 = LINE('',#22871,#2298) ;
#1463 = LINE('',#22875,#2299) ;
#1464 = LINE('',#22877,#2300) ;
#1465 = LINE('',#22879,#2301) ;
#1466 = LINE('',#22880,#2302) ;
#1467 = LINE('',#22883,#2303) ;
#1468 = LINE('',#22885,#2304) ;
#1469 = LINE('',#22886,#2305) ;
#1470 = LINE('',#22889,#2306) ;
#1471 = LINE('',#22890,#2307) ;
#1472 = LINE('',#22893,#2308) ;
#1473 = LINE('',#22894,#2309) ;
#1474 = LINE('',#22896,#2310) ;
#1475 = LINE('',#22900,#2311) ;
#1476 = LINE('',#22902,#2312) ;
#1477 = LINE('',#22904,#2313) ;
#1478 = LINE('',#22905,#2314) ;
#1479 = LINE('',#22909,#2315) ;
#1480 = LINE('',#22911,#2316) ;
#1481 = LINE('',#22913,#2317) ;
#1482 = LINE('',#22914,#2318) ;
#1483 = LINE('',#22916,#2319) ;
#1484 = LINE('',#22917,#2320) ;
#1485 = LINE('',#22919,#2321) ;
#1486 = LINE('',#22921,#2322) ;
#1487 = LINE('',#22927,#2323) ;
#1488 = LINE('',#22929,#2324) ;
#1489 = LINE('',#22931,#2325) ;
#1490 = LINE('',#22933,#2326) ;
#1491 = LINE('',#22935,#2327) ;
#1492 = LINE('',#22937,#2328) ;
#1493 = LINE('',#22939,#2329) ;
#1494 = LINE('',#22940,#2330) ;
#1495 = LINE('',#22944,#2331) ;
#1496 = LINE('',#22946,#2332) ;
#1497 = LINE('',#22948,#2333) ;
#1498 = LINE('',#22949,#2334) ;
#1499 = LINE('',#22954,#2335) ;
#1500 = LINE('',#22956,#2336) ;
#1501 = LINE('',#22958,#2337) ;
#1502 = LINE('',#22959,#2338) ;
#1503 = LINE('',#22964,#2339) ;
#1504 = LINE('',#22966,#2340) ;
#1505 = LINE('',#22968,#2341) ;
#1506 = LINE('',#22969,#2342) ;
#1507 = LINE('',#22973,#2343) ;
#1508 = LINE('',#22974,#2344) ;
#1509 = LINE('',#22976,#2345) ;
#1510 = LINE('',#22979,#2346) ;
#1511 = LINE('',#22983,#2347) ;
#1512 = LINE('',#22989,#2348) ;
#1513 = LINE('',#22993,#2349) ;
#1514 = LINE('',#22996,#2350) ;
#1515 = LINE('',#22997,#2351) ;
#1516 = LINE('',#23000,#2352) ;
#1517 = LINE('',#23002,#2353) ;
#1518 = LINE('',#23006,#2354) ;
#1519 = LINE('',#23008,#2355) ;
#1520 = LINE('',#23009,#2356) ;
#1521 = LINE('',#23012,#2357) ;
#1522 = LINE('',#23017,#2358) ;
#1523 = LINE('',#23025,#2359) ;
#1524 = LINE('',#23032,#2360) ;
#1525 = LINE('',#23090,#2361) ;
#1526 = LINE('',#23096,#2362) ;
#1527 = LINE('',#23102,#2363) ;
#1528 = LINE('',#23123,#2364) ;
#1529 = LINE('',#23148,#2365) ;
#1530 = LINE('',#23153,#2366) ;
#1531 = LINE('',#23155,#2367) ;
#1532 = LINE('',#23157,#2368) ;
#1533 = LINE('',#23158,#2369) ;
#1534 = LINE('',#23162,#2370) ;
#1535 = LINE('',#23164,#2371) ;
#1536 = LINE('',#23166,#2372) ;
#1537 = LINE('',#23167,#2373) ;
#1538 = LINE('',#23169,#2374) ;
#1539 = LINE('',#23170,#2375) ;
#1540 = LINE('',#23172,#2376) ;
#1541 = LINE('',#23174,#2377) ;
#1542 = LINE('',#23181,#2378) ;
#1543 = LINE('',#23188,#2379) ;
#1544 = LINE('',#23191,#2380) ;
#1545 = LINE('',#23225,#2381) ;
#1546 = LINE('',#23229,#2382) ;
#1547 = LINE('',#23233,#2383) ;
#1548 = LINE('',#23237,#2384) ;
#1549 = LINE('',#23241,#2385) ;
#1550 = LINE('',#23245,#2386) ;
#1551 = LINE('',#23249,#2387) ;
#1552 = LINE('',#23253,#2388) ;
#1553 = LINE('',#23257,#2389) ;
#1554 = LINE('',#23261,#2390) ;
#1555 = LINE('',#23265,#2391) ;
#1556 = LINE('',#23269,#2392) ;
#1557 = LINE('',#23273,#2393) ;
#1558 = LINE('',#23277,#2394) ;
#1559 = LINE('',#23286,#2395) ;
#1560 = LINE('',#23295,#2396) ;
#1561 = LINE('',#23301,#2397) ;
#1562 = LINE('',#23310,#2398) ;
#1563 = LINE('',#23316,#2399) ;
#1564 = LINE('',#23324,#2400) ;
#1565 = LINE('',#23326,#2401) ;
#1566 = LINE('',#23327,#2402) ;
#1567 = LINE('',#23330,#2403) ;
#1568 = LINE('',#23332,#2404) ;
#1569 = LINE('',#23333,#2405) ;
#1570 = LINE('',#23336,#2406) ;
#1571 = LINE('',#23338,#2407) ;
#1572 = LINE('',#23339,#2408) ;
#1573 = LINE('',#23342,#2409) ;
#1574 = LINE('',#23349,#2410) ;
#1575 = LINE('',#23351,#2411) ;
#1576 = LINE('',#23352,#2412) ;
#1577 = LINE('',#23355,#2413) ;
#1578 = LINE('',#23357,#2414) ;
#1579 = LINE('',#23358,#2415) ;
#1580 = LINE('',#23361,#2416) ;
#1581 = LINE('',#23363,#2417) ;
#1582 = LINE('',#23364,#2418) ;
#1583 = LINE('',#23367,#2419) ;
#1584 = LINE('',#23374,#2420) ;
#1585 = LINE('',#23376,#2421) ;
#1586 = LINE('',#23377,#2422) ;
#1587 = LINE('',#23380,#2423) ;
#1588 = LINE('',#23382,#2424) ;
#1589 = LINE('',#23383,#2425) ;
#1590 = LINE('',#23386,#2426) ;
#1591 = LINE('',#23388,#2427) ;
#1592 = LINE('',#23389,#2428) ;
#1593 = LINE('',#23392,#2429) ;
#1594 = LINE('',#23399,#2430) ;
#1595 = LINE('',#23401,#2431) ;
#1596 = LINE('',#23402,#2432) ;
#1597 = LINE('',#23405,#2433) ;
#1598 = LINE('',#23407,#2434) ;
#1599 = LINE('',#23408,#2435) ;
#1600 = LINE('',#23411,#2436) ;
#1601 = LINE('',#23413,#2437) ;
#1602 = LINE('',#23414,#2438) ;
#1603 = LINE('',#23417,#2439) ;
#1604 = LINE('',#23424,#2440) ;
#1605 = LINE('',#23426,#2441) ;
#1606 = LINE('',#23428,#2442) ;
#1607 = LINE('',#23432,#2443) ;
#1608 = LINE('',#23434,#2444) ;
#1609 = LINE('',#23435,#2445) ;
#1610 = LINE('',#23438,#2446) ;
#1611 = LINE('',#23440,#2447) ;
#1612 = LINE('',#23441,#2448) ;
#1613 = LINE('',#23445,#2449) ;
#1614 = LINE('',#23453,#2450) ;
#1615 = LINE('',#23455,#2451) ;
#1616 = LINE('',#23456,#2452) ;
#1617 = LINE('',#23459,#2453) ;
#1618 = LINE('',#23461,#2454) ;
#1619 = LINE('',#23462,#2455) ;
#1620 = LINE('',#23465,#2456) ;
#1621 = LINE('',#23467,#2457) ;
#1622 = LINE('',#23468,#2458) ;
#1623 = LINE('',#23471,#2459) ;
#1624 = LINE('',#23478,#2460) ;
#1625 = LINE('',#23480,#2461) ;
#1626 = LINE('',#23481,#2462) ;
#1627 = LINE('',#23484,#2463) ;
#1628 = LINE('',#23486,#2464) ;
#1629 = LINE('',#23487,#2465) ;
#1630 = LINE('',#23490,#2466) ;
#1631 = LINE('',#23492,#2467) ;
#1632 = LINE('',#23493,#2468) ;
#1633 = LINE('',#23496,#2469) ;
#1634 = LINE('',#23503,#2470) ;
#1635 = LINE('',#23505,#2471) ;
#1636 = LINE('',#23506,#2472) ;
#1637 = LINE('',#23509,#2473) ;
#1638 = LINE('',#23511,#2474) ;
#1639 = LINE('',#23512,#2475) ;
#1640 = LINE('',#23515,#2476) ;
#1641 = LINE('',#23517,#2477) ;
#1642 = LINE('',#23518,#2478) ;
#1643 = LINE('',#23521,#2479) ;
#1644 = LINE('',#23528,#2480) ;
#1645 = LINE('',#23530,#2481) ;
#1646 = LINE('',#23531,#2482) ;
#1647 = LINE('',#23534,#2483) ;
#1648 = LINE('',#23536,#2484) ;
#1649 = LINE('',#23537,#2485) ;
#1650 = LINE('',#23540,#2486) ;
#1651 = LINE('',#23542,#2487) ;
#1652 = LINE('',#23543,#2488) ;
#1653 = LINE('',#23546,#2489) ;
#1654 = LINE('',#23553,#2490) ;
#1655 = LINE('',#23555,#2491) ;
#1656 = LINE('',#23556,#2492) ;
#1657 = LINE('',#23559,#2493) ;
#1658 = LINE('',#23561,#2494) ;
#1659 = LINE('',#23562,#2495) ;
#1660 = LINE('',#23565,#2496) ;
#1661 = LINE('',#23567,#2497) ;
#1662 = LINE('',#23568,#2498) ;
#1663 = LINE('',#23571,#2499) ;
#1664 = LINE('',#23576,#2500) ;
#1665 = LINE('',#23578,#2501) ;
#1666 = LINE('',#23587,#2502) ;
#1667 = LINE('',#23593,#2503) ;
#1668 = LINE('',#23601,#2504) ;
#1669 = LINE('',#23605,#2505) ;
#1670 = LINE('',#23610,#2506) ;
#1671 = LINE('',#23614,#2507) ;
#1672 = LINE('',#23616,#2508) ;
#1673 = LINE('',#23618,#2509) ;
#1674 = LINE('',#23654,#2510) ;
#1675 = LINE('',#23686,#2511) ;
#1676 = LINE('',#23690,#2512) ;
#1677 = LINE('',#23694,#2513) ;
#1678 = LINE('',#23699,#2514) ;
#1679 = LINE('',#23705,#2515) ;
#1680 = LINE('',#23707,#2516) ;
#1681 = LINE('',#23709,#2517) ;
#1682 = LINE('',#23710,#2518) ;
#1683 = LINE('',#23714,#2519) ;
#1684 = LINE('',#23716,#2520) ;
#1685 = LINE('',#23718,#2521) ;
#1686 = LINE('',#23719,#2522) ;
#1687 = LINE('',#23723,#2523) ;
#1688 = LINE('',#23725,#2524) ;
#1689 = LINE('',#23727,#2525) ;
#1690 = LINE('',#23728,#2526) ;
#1691 = LINE('',#23730,#2527) ;
#1692 = LINE('',#23731,#2528) ;
#1693 = LINE('',#23744,#2529) ;
#1694 = LINE('',#23746,#2530) ;
#1695 = LINE('',#23748,#2531) ;
#1696 = LINE('',#23749,#2532) ;
#1697 = LINE('',#23753,#2533) ;
#1698 = LINE('',#23755,#2534) ;
#1699 = LINE('',#23757,#2535) ;
#1700 = LINE('',#23758,#2536) ;
#1701 = LINE('',#23762,#2537) ;
#1702 = LINE('',#23764,#2538) ;
#1703 = LINE('',#23766,#2539) ;
#1704 = LINE('',#23767,#2540) ;
#1705 = LINE('',#23769,#2541) ;
#1706 = LINE('',#23770,#2542) ;
#1707 = LINE('',#23826,#2543) ;
#1708 = LINE('',#23912,#2544) ;
#1709 = LINE('',#23914,#2545) ;
#1710 = LINE('',#23919,#2546) ;
#1711 = LINE('',#23921,#2547) ;
#1712 = LINE('',#23929,#2548) ;
#1713 = LINE('',#23933,#2549) ;
#1714 = LINE('',#24064,#2550) ;
#1715 = LINE('',#24065,#2551) ;
#1716 = LINE('',#24069,#2552) ;
#1717 = LINE('',#24071,#2553) ;
#1718 = LINE('',#24077,#2554) ;
#1719 = LINE('',#24081,#2555) ;
#1720 = LINE('',#24083,#2556) ;
#1721 = LINE('',#24087,#2557) ;
#1722 = LINE('',#24095,#2558) ;
#1723 = LINE('',#24101,#2559) ;
#1724 = LINE('',#24110,#2560) ;
#1725 = LINE('',#24116,#2561) ;
#1726 = LINE('',#24122,#2562) ;
#1727 = LINE('',#24128,#2563) ;
#1728 = LINE('',#24134,#2564) ;
#1729 = LINE('',#24140,#2565) ;
#1730 = LINE('',#24149,#2566) ;
#1731 = LINE('',#24155,#2567) ;
#1732 = LINE('',#24161,#2568) ;
#1733 = LINE('',#24167,#2569) ;
#1734 = LINE('',#24173,#2570) ;
#1735 = LINE('',#24179,#2571) ;
#1736 = LINE('',#24187,#2572) ;
#1737 = LINE('',#24193,#2573) ;
#1738 = LINE('',#24218,#2574) ;
#1739 = LINE('',#24224,#2575) ;
#1740 = LINE('',#24248,#2576) ;
#1741 = LINE('',#24250,#2577) ;
#1742 = LINE('',#24252,#2578) ;
#1743 = LINE('',#24253,#2579) ;
#1744 = LINE('',#24257,#2580) ;
#1745 = LINE('',#24259,#2581) ;
#1746 = LINE('',#24261,#2582) ;
#1747 = LINE('',#24262,#2583) ;
#1748 = LINE('',#24266,#2584) ;
#1749 = LINE('',#24268,#2585) ;
#1750 = LINE('',#24270,#2586) ;
#1751 = LINE('',#24271,#2587) ;
#1752 = LINE('',#24273,#2588) ;
#1753 = LINE('',#24274,#2589) ;
#1754 = LINE('',#24276,#2590) ;
#1755 = LINE('',#24277,#2591) ;
#1756 = LINE('',#24286,#2592) ;
#1757 = LINE('',#24302,#2593) ;
#1758 = LINE('',#24309,#2594) ;
#1759 = LINE('',#24318,#2595) ;
#1760 = LINE('',#24324,#2596) ;
#1761 = LINE('',#24333,#2597) ;
#1762 = LINE('',#24338,#2598) ;
#1763 = LINE('',#24340,#2599) ;
#1764 = LINE('',#24342,#2600) ;
#1765 = LINE('',#24343,#2601) ;
#1766 = LINE('',#24347,#2602) ;
#1767 = LINE('',#24349,#2603) ;
#1768 = LINE('',#24351,#2604) ;
#1769 = LINE('',#24352,#2605) ;
#1770 = LINE('',#24355,#2606) ;
#1771 = LINE('',#24356,#2607) ;
#1772 = LINE('',#24358,#2608) ;
#1773 = LINE('',#24359,#2609) ;
#1774 = LINE('',#24362,#2610) ;
#1775 = LINE('',#24363,#2611) ;
#1776 = LINE('',#24366,#2612) ;
#1777 = LINE('',#24367,#2613) ;
#1778 = LINE('',#24369,#2614) ;
#1779 = LINE('',#24371,#2615) ;
#1780 = LINE('',#24378,#2616) ;
#1781 = LINE('',#24384,#2617) ;
#1782 = LINE('',#24386,#2618) ;
#1783 = LINE('',#24388,#2619) ;
#1784 = LINE('',#24389,#2620) ;
#1785 = LINE('',#24393,#2621) ;
#1786 = LINE('',#24395,#2622) ;
#1787 = LINE('',#24397,#2623) ;
#1788 = LINE('',#24398,#2624) ;
#1789 = LINE('',#24401,#2625) ;
#1790 = LINE('',#24402,#2626) ;
#1791 = LINE('',#24404,#2627) ;
#1792 = LINE('',#24405,#2628) ;
#1793 = LINE('',#24408,#2629) ;
#1794 = LINE('',#24409,#2630) ;
#1795 = LINE('',#24412,#2631) ;
#1796 = LINE('',#24413,#2632) ;
#1797 = LINE('',#24415,#2633) ;
#1798 = LINE('',#24417,#2634) ;
#1799 = LINE('',#24424,#2635) ;
#1800 = LINE('',#24430,#2636) ;
#1801 = LINE('',#24432,#2637) ;
#1802 = LINE('',#24434,#2638) ;
#1803 = LINE('',#24435,#2639) ;
#1804 = LINE('',#24439,#2640) ;
#1805 = LINE('',#24441,#2641) ;
#1806 = LINE('',#24443,#2642) ;
#1807 = LINE('',#24444,#2643) ;
#1808 = LINE('',#24447,#2644) ;
#1809 = LINE('',#24448,#2645) ;
#1810 = LINE('',#24450,#2646) ;
#1811 = LINE('',#24451,#2647) ;
#1812 = LINE('',#24454,#2648) ;
#1813 = LINE('',#24455,#2649) ;
#1814 = LINE('',#24458,#2650) ;
#1815 = LINE('',#24459,#2651) ;
#1816 = LINE('',#24461,#2652) ;
#1817 = LINE('',#24463,#2653) ;
#1818 = LINE('',#24470,#2654) ;
#1819 = LINE('',#24475,#2655) ;
#1820 = LINE('',#24477,#2656) ;
#1821 = LINE('',#24479,#2657) ;
#1822 = LINE('',#24480,#2658) ;
#1823 = LINE('',#24484,#2659) ;
#1824 = LINE('',#24486,#2660) ;
#1825 = LINE('',#24488,#2661) ;
#1826 = LINE('',#24489,#2662) ;
#1827 = LINE('',#24492,#2663) ;
#1828 = LINE('',#24493,#2664) ;
#1829 = LINE('',#24495,#2665) ;
#1830 = LINE('',#24496,#2666) ;
#1831 = LINE('',#24499,#2667) ;
#1832 = LINE('',#24500,#2668) ;
#1833 = LINE('',#24503,#2669) ;
#1834 = LINE('',#24504,#2670) ;
#1835 = LINE('',#24506,#2671) ;
#1836 = LINE('',#24508,#2672) ;
#1837 = VECTOR('',#15408,0.41) ;
#1838 = VECTOR('',#15409,1.) ;
#1839 = VECTOR('',#15412,1.) ;
#1840 = VECTOR('',#15417,1.) ;
#1841 = VECTOR('',#15420,1.) ;
#1842 = VECTOR('',#15423,11.4) ;
#1843 = VECTOR('',#15428,1.) ;
#1844 = VECTOR('',#15431,1.) ;
#1845 = VECTOR('',#15434,1.) ;
#1846 = VECTOR('',#15435,1.) ;
#1847 = VECTOR('',#15440,0.41) ;
#1848 = VECTOR('',#15461,0.325) ;
#1849 = VECTOR('',#15468,0.325) ;
#1850 = VECTOR('',#15475,0.325) ;
#1851 = VECTOR('',#15482,0.325) ;
#1852 = VECTOR('',#15489,0.325) ;
#1853 = VECTOR('',#15496,0.325) ;
#1854 = VECTOR('',#15501,1.) ;
#1855 = VECTOR('',#15502,1.) ;
#1856 = VECTOR('',#15503,1.) ;
#1857 = VECTOR('',#15504,1.) ;
#1858 = VECTOR('',#15505,1.) ;
#1859 = VECTOR('',#15506,1.) ;
#1860 = VECTOR('',#15509,1.) ;
#1861 = VECTOR('',#15510,1.) ;
#1862 = VECTOR('',#15511,1.) ;
#1863 = VECTOR('',#15516,1.) ;
#1864 = VECTOR('',#15519,1.) ;
#1865 = VECTOR('',#15520,1.) ;
#1866 = VECTOR('',#15521,1.) ;
#1867 = VECTOR('',#15524,1.) ;
#1868 = VECTOR('',#15529,1.) ;
#1869 = VECTOR('',#15532,1.) ;
#1870 = VECTOR('',#15533,1.) ;
#1871 = VECTOR('',#15538,12.5) ;
#1872 = VECTOR('',#15543,1.) ;
#1873 = VECTOR('',#15546,1.) ;
#1874 = VECTOR('',#15553,1.1) ;
#1875 = VECTOR('',#15558,1.5) ;
#1876 = VECTOR('',#15577,0.9) ;
#1877 = VECTOR('',#15586,1.2) ;
#1878 = VECTOR('',#15601,1.5) ;
#1879 = VECTOR('',#15608,1.75) ;
#1880 = VECTOR('',#15617,1.75) ;
#1881 = VECTOR('',#15626,2.5) ;
#1882 = VECTOR('',#15631,2.5) ;
#1883 = VECTOR('',#15644,0.2025) ;
#1884 = VECTOR('',#15651,0.325) ;
#1885 = VECTOR('',#15658,0.325) ;
#1886 = VECTOR('',#15665,0.325) ;
#1887 = VECTOR('',#15672,0.325) ;
#1888 = VECTOR('',#15679,0.325) ;
#1889 = VECTOR('',#15686,0.325) ;
#1890 = VECTOR('',#15693,1.41) ;
#1891 = VECTOR('',#15700,1.8) ;
#1892 = VECTOR('',#15709,1.41) ;
#1893 = VECTOR('',#15716,1.8) ;
#1894 = VECTOR('',#15725,5.9) ;
#1895 = VECTOR('',#15736,5.5) ;
#1896 = VECTOR('',#15741,11.4) ;
#1897 = VECTOR('',#15750,12.5) ;
#1898 = VECTOR('',#15763,5.89) ;
#1899 = VECTOR('',#15776,0.325) ;
#1900 = VECTOR('',#15783,0.325) ;
#1901 = VECTOR('',#15790,0.325) ;
#1902 = VECTOR('',#15797,0.325) ;
#1903 = VECTOR('',#15804,0.325) ;
#1904 = VECTOR('',#15811,0.325) ;
#1905 = VECTOR('',#15818,11.4) ;
#1906 = VECTOR('',#15825,12.5) ;
#1907 = VECTOR('',#15836,1.) ;
#1908 = VECTOR('',#15837,1.) ;
#1909 = VECTOR('',#15838,1.) ;
#1910 = VECTOR('',#15839,1.) ;
#1911 = VECTOR('',#15844,1.) ;
#1912 = VECTOR('',#15845,1.) ;
#1913 = VECTOR('',#15848,1.) ;
#1914 = VECTOR('',#15849,1.) ;
#1915 = VECTOR('',#15850,1.) ;
#1916 = VECTOR('',#15853,1.) ;
#1917 = VECTOR('',#15858,0.75) ;
#1918 = VECTOR('',#15867,0.7) ;
#1919 = VECTOR('',#15880,0.75) ;
#1920 = VECTOR('',#15885,0.195) ;
#1921 = VECTOR('',#15892,0.195) ;
#1922 = VECTOR('',#15899,0.195) ;
#1923 = VECTOR('',#15910,2.5) ;
#1924 = VECTOR('',#15915,0.5) ;
#1925 = VECTOR('',#15930,0.15) ;
#1926 = VECTOR('',#15939,0.15) ;
#1927 = VECTOR('',#15948,0.15) ;
#1928 = VECTOR('',#15957,0.15) ;
#1929 = VECTOR('',#15966,0.15) ;
#1930 = VECTOR('',#15975,0.15) ;
#1931 = VECTOR('',#15984,0.15) ;
#1932 = VECTOR('',#15993,0.15) ;
#1933 = VECTOR('',#16002,0.15) ;
#1934 = VECTOR('',#16011,0.15) ;
#1935 = VECTOR('',#16020,0.15) ;
#1936 = VECTOR('',#16029,0.15) ;
#1937 = VECTOR('',#16038,0.15) ;
#1938 = VECTOR('',#16047,0.15) ;
#1939 = VECTOR('',#16056,0.15) ;
#1940 = VECTOR('',#16065,0.15) ;
#1941 = VECTOR('',#16074,0.15) ;
#1942 = VECTOR('',#16083,0.15) ;
#1943 = VECTOR('',#16092,0.15) ;
#1944 = VECTOR('',#16101,0.15) ;
#1945 = VECTOR('',#16110,0.15) ;
#1946 = VECTOR('',#16119,0.15) ;
#1947 = VECTOR('',#16128,0.15) ;
#1948 = VECTOR('',#16137,0.15) ;
#1949 = VECTOR('',#16146,0.4) ;
#1950 = VECTOR('',#16153,0.4) ;
#1951 = VECTOR('',#16160,0.4) ;
#1952 = VECTOR('',#16167,0.4) ;
#1953 = VECTOR('',#16174,0.4) ;
#1954 = VECTOR('',#16181,0.4) ;
#1955 = VECTOR('',#16188,0.4) ;
#1956 = VECTOR('',#16195,0.4) ;
#1957 = VECTOR('',#16202,0.4) ;
#1958 = VECTOR('',#16209,0.4) ;
#1959 = VECTOR('',#16216,0.4) ;
#1960 = VECTOR('',#16223,0.4) ;
#1961 = VECTOR('',#16230,0.4) ;
#1962 = VECTOR('',#16237,0.4) ;
#1963 = VECTOR('',#16244,0.4) ;
#1964 = VECTOR('',#16251,0.4) ;
#1965 = VECTOR('',#16258,0.4) ;
#1966 = VECTOR('',#16265,0.4) ;
#1967 = VECTOR('',#16272,0.4) ;
#1968 = VECTOR('',#16279,0.4) ;
#1969 = VECTOR('',#16286,0.4) ;
#1970 = VECTOR('',#16293,0.4) ;
#1971 = VECTOR('',#16300,0.4) ;
#1972 = VECTOR('',#16307,0.4) ;
#1973 = VECTOR('',#16314,0.215) ;
#1974 = VECTOR('',#16321,0.215) ;
#1975 = VECTOR('',#16328,0.215) ;
#1976 = VECTOR('',#16335,0.51) ;
#1977 = VECTOR('',#16342,10.) ;
#1978 = VECTOR('',#16365,1.05) ;
#1979 = VECTOR('',#16368,1.45) ;
#1980 = VECTOR('',#16379,1.75) ;
#1981 = VECTOR('',#16386,0.75) ;
#1982 = VECTOR('',#16403,1.05) ;
#1983 = VECTOR('',#16406,1.45) ;
#1984 = VECTOR('',#16417,1.75) ;
#1985 = VECTOR('',#16424,0.75) ;
#1986 = VECTOR('',#16431,0.75) ;
#1987 = VECTOR('',#16438,1.1) ;
#1988 = VECTOR('',#16449,1.) ;
#1989 = VECTOR('',#16450,1.) ;
#1990 = VECTOR('',#16451,1.) ;
#1991 = VECTOR('',#16452,1.) ;
#1992 = VECTOR('',#16455,1.) ;
#1993 = VECTOR('',#16456,1.) ;
#1994 = VECTOR('',#16457,1.) ;
#1995 = VECTOR('',#16458,1.) ;
#1996 = VECTOR('',#16479,1.) ;
#1997 = VECTOR('',#16480,1.) ;
#1998 = VECTOR('',#16481,1.) ;
#1999 = VECTOR('',#16482,1.) ;
#2000 = VECTOR('',#16485,1.) ;
#2001 = VECTOR('',#16486,1.) ;
#2002 = VECTOR('',#16487,1.) ;
#2003 = VECTOR('',#16488,1.) ;
#2004 = VECTOR('',#16491,1.) ;
#2005 = VECTOR('',#16492,1.) ;
#2006 = VECTOR('',#16505,1.) ;
#2007 = VECTOR('',#16506,1.) ;
#2008 = VECTOR('',#16507,1.) ;
#2009 = VECTOR('',#16508,1.) ;
#2010 = VECTOR('',#16511,1.) ;
#2011 = VECTOR('',#16512,1.) ;
#2012 = VECTOR('',#16513,1.) ;
#2013 = VECTOR('',#16514,1.) ;
#2014 = VECTOR('',#16517,1.) ;
#2015 = VECTOR('',#16518,1.) ;
#2016 = VECTOR('',#16523,1.) ;
#2017 = VECTOR('',#16530,1.) ;
#2018 = VECTOR('',#16535,1.) ;
#2019 = VECTOR('',#16536,1.) ;
#2020 = VECTOR('',#16537,1.) ;
#2021 = VECTOR('',#16540,1.) ;
#2022 = VECTOR('',#16541,1.) ;
#2023 = VECTOR('',#16542,1.) ;
#2024 = VECTOR('',#16545,1.) ;
#2025 = VECTOR('',#16546,1.) ;
#2026 = VECTOR('',#16547,1.) ;
#2027 = VECTOR('',#16550,1.) ;
#2028 = VECTOR('',#16551,1.) ;
#2029 = VECTOR('',#16552,1.) ;
#2030 = VECTOR('',#16555,1.) ;
#2031 = VECTOR('',#16556,1.) ;
#2032 = VECTOR('',#16557,1.) ;
#2033 = VECTOR('',#16560,1.) ;
#2034 = VECTOR('',#16561,1.) ;
#2035 = VECTOR('',#16562,1.) ;
#2036 = VECTOR('',#16565,1.) ;
#2037 = VECTOR('',#16566,1.) ;
#2038 = VECTOR('',#16567,1.) ;
#2039 = VECTOR('',#16570,1.) ;
#2040 = VECTOR('',#16571,1.) ;
#2041 = VECTOR('',#16572,1.) ;
#2042 = VECTOR('',#16575,1.) ;
#2043 = VECTOR('',#16576,1.) ;
#2044 = VECTOR('',#16577,1.) ;
#2045 = VECTOR('',#16580,1.) ;
#2046 = VECTOR('',#16581,1.) ;
#2047 = VECTOR('',#16582,1.) ;
#2048 = VECTOR('',#16585,1.) ;
#2049 = VECTOR('',#16586,1.) ;
#2050 = VECTOR('',#16587,1.) ;
#2051 = VECTOR('',#16590,1.) ;
#2052 = VECTOR('',#16591,1.) ;
#2053 = VECTOR('',#16594,1.) ;
#2054 = VECTOR('',#16595,1.) ;
#2055 = VECTOR('',#16596,1.) ;
#2056 = VECTOR('',#16599,1.) ;
#2057 = VECTOR('',#16604,1.) ;
#2058 = VECTOR('',#16607,1.) ;
#2059 = VECTOR('',#16608,1.) ;
#2060 = VECTOR('',#16609,1.) ;
#2061 = VECTOR('',#16612,1.) ;
#2062 = VECTOR('',#16613,1.) ;
#2063 = VECTOR('',#16616,1.) ;
#2064 = VECTOR('',#16621,1.) ;
#2065 = VECTOR('',#16624,1.) ;
#2066 = VECTOR('',#16625,1.) ;
#2067 = VECTOR('',#16628,1.) ;
#2068 = VECTOR('',#16629,1.) ;
#2069 = VECTOR('',#16630,1.) ;
#2070 = VECTOR('',#16633,1.) ;
#2071 = VECTOR('',#16638,1.) ;
#2072 = VECTOR('',#16641,1.) ;
#2073 = VECTOR('',#16642,1.) ;
#2074 = VECTOR('',#16643,1.) ;
#2075 = VECTOR('',#16646,1.) ;
#2076 = VECTOR('',#16647,1.) ;
#2077 = VECTOR('',#16650,1.) ;
#2078 = VECTOR('',#16655,1.) ;
#2079 = VECTOR('',#16658,1.) ;
#2080 = VECTOR('',#16659,1.) ;
#2081 = VECTOR('',#16662,1.) ;
#2082 = VECTOR('',#16663,1.) ;
#2083 = VECTOR('',#16664,1.) ;
#2084 = VECTOR('',#16667,1.) ;
#2085 = VECTOR('',#16672,1.) ;
#2086 = VECTOR('',#16675,1.) ;
#2087 = VECTOR('',#16676,1.) ;
#2088 = VECTOR('',#16677,1.) ;
#2089 = VECTOR('',#16680,1.) ;
#2090 = VECTOR('',#16681,1.) ;
#2091 = VECTOR('',#16684,1.) ;
#2092 = VECTOR('',#16689,1.) ;
#2093 = VECTOR('',#16692,1.) ;
#2094 = VECTOR('',#16693,1.) ;
#2095 = VECTOR('',#16696,1.) ;
#2096 = VECTOR('',#16697,1.) ;
#2097 = VECTOR('',#16698,1.) ;
#2098 = VECTOR('',#16701,1.) ;
#2099 = VECTOR('',#16706,1.) ;
#2100 = VECTOR('',#16709,1.) ;
#2101 = VECTOR('',#16710,1.) ;
#2102 = VECTOR('',#16711,1.) ;
#2103 = VECTOR('',#16714,1.) ;
#2104 = VECTOR('',#16715,1.) ;
#2105 = VECTOR('',#16718,1.) ;
#2106 = VECTOR('',#16723,1.) ;
#2107 = VECTOR('',#16726,1.) ;
#2108 = VECTOR('',#16727,1.) ;
#2109 = VECTOR('',#16730,1.) ;
#2110 = VECTOR('',#16731,1.) ;
#2111 = VECTOR('',#16732,1.) ;
#2112 = VECTOR('',#16735,1.) ;
#2113 = VECTOR('',#16740,1.) ;
#2114 = VECTOR('',#16743,1.) ;
#2115 = VECTOR('',#16744,1.) ;
#2116 = VECTOR('',#16745,1.) ;
#2117 = VECTOR('',#16748,1.) ;
#2118 = VECTOR('',#16749,1.) ;
#2119 = VECTOR('',#16752,1.) ;
#2120 = VECTOR('',#16757,1.) ;
#2121 = VECTOR('',#16760,1.) ;
#2122 = VECTOR('',#16761,1.) ;
#2123 = VECTOR('',#16764,1.) ;
#2124 = VECTOR('',#16765,1.) ;
#2125 = VECTOR('',#16768,1.) ;
#2126 = VECTOR('',#16773,1.4) ;
#2127 = VECTOR('',#16780,1.) ;
#2128 = VECTOR('',#16781,1.) ;
#2129 = VECTOR('',#16782,1.) ;
#2130 = VECTOR('',#16783,1.) ;
#2131 = VECTOR('',#16786,1.) ;
#2132 = VECTOR('',#16787,1.) ;
#2133 = VECTOR('',#16788,1.) ;
#2134 = VECTOR('',#16789,1.) ;
#2135 = VECTOR('',#16792,1.) ;
#2136 = VECTOR('',#16793,1.) ;
#2137 = VECTOR('',#16796,1.) ;
#2138 = VECTOR('',#16799,1.) ;
#2139 = VECTOR('',#16808,10.2) ;
#2140 = VECTOR('',#16815,11.1) ;
#2141 = VECTOR('',#16826,1.) ;
#2142 = VECTOR('',#16827,1.) ;
#2143 = VECTOR('',#16828,1.) ;
#2144 = VECTOR('',#16829,1.) ;
#2145 = VECTOR('',#16832,1.) ;
#2146 = VECTOR('',#16833,1.) ;
#2147 = VECTOR('',#16834,1.) ;
#2148 = VECTOR('',#16837,1.) ;
#2149 = VECTOR('',#16838,1.) ;
#2150 = VECTOR('',#16841,1.) ;
#2151 = VECTOR('',#16842,1.) ;
#2152 = VECTOR('',#16845,1.) ;
#2153 = VECTOR('',#16846,1.) ;
#2154 = VECTOR('',#16847,1.) ;
#2155 = VECTOR('',#16848,1.) ;
#2156 = VECTOR('',#16849,1.) ;
#2157 = VECTOR('',#16852,1.) ;
#2158 = VECTOR('',#16853,1.) ;
#2159 = VECTOR('',#16854,1.) ;
#2160 = VECTOR('',#16857,1.) ;
#2161 = VECTOR('',#16858,1.) ;
#2162 = VECTOR('',#16859,1.) ;
#2163 = VECTOR('',#16862,1.) ;
#2164 = VECTOR('',#16863,1.) ;
#2165 = VECTOR('',#16874,0.25) ;
#2166 = VECTOR('',#16883,0.21) ;
#2167 = VECTOR('',#16888,1.) ;
#2168 = VECTOR('',#16891,1.) ;
#2169 = VECTOR('',#16896,1.) ;
#2170 = VECTOR('',#16899,1.) ;
#2171 = VECTOR('',#16904,1.) ;
#2172 = VECTOR('',#16907,1.) ;
#2173 = VECTOR('',#16912,1.) ;
#2174 = VECTOR('',#16913,1.) ;
#2175 = VECTOR('',#16914,1.) ;
#2176 = VECTOR('',#16917,1.) ;
#2177 = VECTOR('',#16918,1.) ;
#2178 = VECTOR('',#16919,1.) ;
#2179 = VECTOR('',#16922,1.) ;
#2180 = VECTOR('',#16923,1.) ;
#2181 = VECTOR('',#16924,1.) ;
#2182 = VECTOR('',#16927,1.) ;
#2183 = VECTOR('',#16928,1.) ;
#2184 = VECTOR('',#16929,1.) ;
#2185 = VECTOR('',#16930,1.) ;
#2186 = VECTOR('',#16933,1.) ;
#2187 = VECTOR('',#16936,1.) ;
#2188 = VECTOR('',#16937,1.) ;
#2189 = VECTOR('',#16940,1.) ;
#2190 = VECTOR('',#16941,1.) ;
#2191 = VECTOR('',#16952,0.2) ;
#2192 = VECTOR('',#17247,0.05) ;
#2193 = VECTOR('',#17258,0.05) ;
#2194 = VECTOR('',#17265,0.05) ;
#2195 = VECTOR('',#17270,0.05) ;
#2196 = VECTOR('',#17275,0.05) ;
#2197 = VECTOR('',#17280,0.05) ;
#2198 = VECTOR('',#17287,0.05) ;
#2199 = VECTOR('',#17296,0.05) ;
#2200 = VECTOR('',#17303,0.05) ;
#2201 = VECTOR('',#17312,0.05) ;
#2202 = VECTOR('',#17319,0.05) ;
#2203 = VECTOR('',#17324,0.05) ;
#2204 = VECTOR('',#17329,0.05) ;
#2205 = VECTOR('',#17334,0.05) ;
#2206 = VECTOR('',#17341,0.05) ;
#2207 = VECTOR('',#17350,0.05) ;
#2208 = VECTOR('',#17357,0.05) ;
#2209 = VECTOR('',#17366,0.05) ;
#2210 = VECTOR('',#17373,0.05) ;
#2211 = VECTOR('',#17378,0.05) ;
#2212 = VECTOR('',#17383,0.05) ;
#2213 = VECTOR('',#17388,0.05) ;
#2214 = VECTOR('',#17395,0.05) ;
#2215 = VECTOR('',#17404,0.05) ;
#2216 = VECTOR('',#17411,0.05) ;
#2217 = VECTOR('',#17420,0.05) ;
#2218 = VECTOR('',#17427,0.05) ;
#2219 = VECTOR('',#17432,0.05) ;
#2220 = VECTOR('',#17437,0.05) ;
#2221 = VECTOR('',#17442,0.05) ;
#2222 = VECTOR('',#17449,0.05) ;
#2223 = VECTOR('',#17458,0.05) ;
#2224 = VECTOR('',#17855,1.1) ;
#2225 = VECTOR('',#17860,1.4) ;
#2226 = VECTOR('',#17875,1.4) ;
#2227 = VECTOR('',#17892,1.4) ;
#2228 = VECTOR('',#17899,1.4) ;
#2229 = VECTOR('',#17904,1.4) ;
#2230 = VECTOR('',#17915,1.4) ;
#2231 = VECTOR('',#17928,1.4) ;
#2232 = VECTOR('',#17935,1.4) ;
#2233 = VECTOR('',#17940,1.4) ;
#2234 = VECTOR('',#17951,1.4) ;
#2235 = VECTOR('',#17964,1.4) ;
#2236 = VECTOR('',#17971,1.4) ;
#2237 = VECTOR('',#17976,1.4) ;
#2238 = VECTOR('',#17987,1.4) ;
#2239 = VECTOR('',#18000,1.4) ;
#2240 = VECTOR('',#18011,1.4) ;
#2241 = VECTOR('',#18036,1.1) ;
#2242 = VECTOR('',#18101,1.) ;
#2243 = VECTOR('',#18104,1.) ;
#2244 = VECTOR('',#18107,1.) ;
#2245 = VECTOR('',#18108,1.) ;
#2246 = VECTOR('',#18109,1.) ;
#2247 = VECTOR('',#18116,1.) ;
#2248 = VECTOR('',#18119,1.) ;
#2249 = VECTOR('',#18120,1.) ;
#2250 = VECTOR('',#18125,0.425) ;
#2251 = VECTOR('',#18132,1.) ;
#2252 = VECTOR('',#18135,1.) ;
#2253 = VECTOR('',#18138,1.) ;
#2254 = VECTOR('',#18139,1.) ;
#2255 = VECTOR('',#18140,1.) ;
#2256 = VECTOR('',#18147,1.) ;
#2257 = VECTOR('',#18150,1.) ;
#2258 = VECTOR('',#18151,1.) ;
#2259 = VECTOR('',#18156,0.425) ;
#2260 = VECTOR('',#18161,1.) ;
#2261 = VECTOR('',#18162,1.) ;
#2262 = VECTOR('',#18163,1.) ;
#2263 = VECTOR('',#18164,1.) ;
#2264 = VECTOR('',#18167,1.) ;
#2265 = VECTOR('',#18168,1.) ;
#2266 = VECTOR('',#18169,1.) ;
#2267 = VECTOR('',#18172,1.) ;
#2268 = VECTOR('',#18173,1.) ;
#2269 = VECTOR('',#18174,1.) ;
#2270 = VECTOR('',#18177,1.) ;
#2271 = VECTOR('',#18178,1.) ;
#2272 = VECTOR('',#18179,1.) ;
#2273 = VECTOR('',#18182,1.) ;
#2274 = VECTOR('',#18183,1.) ;
#2275 = VECTOR('',#18186,1.) ;
#2276 = VECTOR('',#18187,1.) ;
#2277 = VECTOR('',#18190,1.) ;
#2278 = VECTOR('',#18253,1.) ;
#2279 = VECTOR('',#18254,1.) ;
#2280 = VECTOR('',#18255,1.) ;
#2281 = VECTOR('',#18256,1.) ;
#2282 = VECTOR('',#18257,16.7569118395806) ;
#2283 = VECTOR('',#18258,16.7569118395806) ;
#2284 = VECTOR('',#18259,16.7569118395806) ;
#2285 = VECTOR('',#18260,16.7569118395806) ;
#2286 = VECTOR('',#18267,0.7) ;
#2287 = VECTOR('',#18274,1.) ;
#2288 = VECTOR('',#18275,1.) ;
#2289 = VECTOR('',#18276,1.) ;
#2290 = VECTOR('',#18277,1.) ;
#2291 = VECTOR('',#18280,1.) ;
#2292 = VECTOR('',#18281,1.) ;
#2293 = VECTOR('',#18282,1.) ;
#2294 = VECTOR('',#18285,1.) ;
#2295 = VECTOR('',#18286,1.) ;
#2296 = VECTOR('',#18289,1.) ;
#2297 = VECTOR('',#18290,1.) ;
#2298 = VECTOR('',#18293,1.) ;
#2299 = VECTOR('',#18296,1.) ;
#2300 = VECTOR('',#18297,1.) ;
#2301 = VECTOR('',#18298,1.) ;
#2302 = VECTOR('',#18299,1.) ;
#2303 = VECTOR('',#18302,1.) ;
#2304 = VECTOR('',#18303,1.) ;
#2305 = VECTOR('',#18304,1.) ;
#2306 = VECTOR('',#18307,1.) ;
#2307 = VECTOR('',#18308,1.) ;
#2308 = VECTOR('',#18311,1.) ;
#2309 = VECTOR('',#18312,1.) ;
#2310 = VECTOR('',#18315,1.) ;
#2311 = VECTOR('',#18318,1.) ;
#2312 = VECTOR('',#18319,1.) ;
#2313 = VECTOR('',#18320,1.) ;
#2314 = VECTOR('',#18321,1.) ;
#2315 = VECTOR('',#18324,1.) ;
#2316 = VECTOR('',#18325,1.) ;
#2317 = VECTOR('',#18326,1.) ;
#2318 = VECTOR('',#18327,1.) ;
#2319 = VECTOR('',#18330,1.) ;
#2320 = VECTOR('',#18331,1.) ;
#2321 = VECTOR('',#18334,1.) ;
#2322 = VECTOR('',#18337,1.) ;
#2323 = VECTOR('',#18344,1.) ;
#2324 = VECTOR('',#18345,1.) ;
#2325 = VECTOR('',#18346,1.) ;
#2326 = VECTOR('',#18347,1.) ;
#2327 = VECTOR('',#18348,1.) ;
#2328 = VECTOR('',#18349,1.) ;
#2329 = VECTOR('',#18350,1.) ;
#2330 = VECTOR('',#18351,1.) ;
#2331 = VECTOR('',#18354,1.) ;
#2332 = VECTOR('',#18355,1.) ;
#2333 = VECTOR('',#18356,1.) ;
#2334 = VECTOR('',#18357,1.) ;
#2335 = VECTOR('',#18362,1.) ;
#2336 = VECTOR('',#18363,1.) ;
#2337 = VECTOR('',#18364,1.) ;
#2338 = VECTOR('',#18365,1.) ;
#2339 = VECTOR('',#18370,1.) ;
#2340 = VECTOR('',#18371,1.) ;
#2341 = VECTOR('',#18372,1.) ;
#2342 = VECTOR('',#18373,1.) ;
#2343 = VECTOR('',#18376,1.) ;
#2344 = VECTOR('',#18377,1.) ;
#2345 = VECTOR('',#18378,1.) ;
#2346 = VECTOR('',#18381,1.) ;
#2347 = VECTOR('',#18386,1.) ;
#2348 = VECTOR('',#18395,1.) ;
#2349 = VECTOR('',#18400,1.) ;
#2350 = VECTOR('',#18403,1.) ;
#2351 = VECTOR('',#18404,1.) ;
#2352 = VECTOR('',#18407,1.) ;
#2353 = VECTOR('',#18408,1.) ;
#2354 = VECTOR('',#18413,1.) ;
#2355 = VECTOR('',#18414,1.) ;
#2356 = VECTOR('',#18415,1.) ;
#2357 = VECTOR('',#18418,1.) ;
#2358 = VECTOR('',#18425,1.) ;
#2359 = VECTOR('',#18436,1.) ;
#2360 = VECTOR('',#18445,1.3) ;
#2361 = VECTOR('',#18450,0.6) ;
#2362 = VECTOR('',#18457,0.6) ;
#2363 = VECTOR('',#18464,1.6) ;
#2364 = VECTOR('',#18467,1.) ;
#2365 = VECTOR('',#18478,1.8) ;
#2366 = VECTOR('',#18483,1.) ;
#2367 = VECTOR('',#18484,1.) ;
#2368 = VECTOR('',#18485,1.) ;
#2369 = VECTOR('',#18486,1.) ;
#2370 = VECTOR('',#18489,1.) ;
#2371 = VECTOR('',#18490,1.) ;
#2372 = VECTOR('',#18491,1.) ;
#2373 = VECTOR('',#18492,1.) ;
#2374 = VECTOR('',#18495,1.) ;
#2375 = VECTOR('',#18496,1.) ;
#2376 = VECTOR('',#18499,1.) ;
#2377 = VECTOR('',#18502,1.) ;
#2378 = VECTOR('',#18511,0.4) ;
#2379 = VECTOR('',#18518,1.) ;
#2380 = VECTOR('',#18521,1.) ;
#2381 = VECTOR('',#18558,1.) ;
#2382 = VECTOR('',#18563,1.) ;
#2383 = VECTOR('',#18568,1.) ;
#2384 = VECTOR('',#18573,1.) ;
#2385 = VECTOR('',#18578,1.) ;
#2386 = VECTOR('',#18583,1.) ;
#2387 = VECTOR('',#18588,1.) ;
#2388 = VECTOR('',#18593,1.) ;
#2389 = VECTOR('',#18598,1.) ;
#2390 = VECTOR('',#18603,1.) ;
#2391 = VECTOR('',#18608,1.) ;
#2392 = VECTOR('',#18613,1.) ;
#2393 = VECTOR('',#18618,1.) ;
#2394 = VECTOR('',#18623,1.) ;
#2395 = VECTOR('',#18636,0.4) ;
#2396 = VECTOR('',#18649,0.4) ;
#2397 = VECTOR('',#18656,0.6) ;
#2398 = VECTOR('',#18669,0.4) ;
#2399 = VECTOR('',#18676,0.8) ;
#2400 = VECTOR('',#18685,1.) ;
#2401 = VECTOR('',#18686,1.) ;
#2402 = VECTOR('',#18687,1.) ;
#2403 = VECTOR('',#18690,1.) ;
#2404 = VECTOR('',#18691,1.) ;
#2405 = VECTOR('',#18692,1.) ;
#2406 = VECTOR('',#18695,1.) ;
#2407 = VECTOR('',#18696,1.) ;
#2408 = VECTOR('',#18697,1.) ;
#2409 = VECTOR('',#18702,1.) ;
#2410 = VECTOR('',#18709,1.) ;
#2411 = VECTOR('',#18710,1.) ;
#2412 = VECTOR('',#18711,1.) ;
#2413 = VECTOR('',#18714,1.) ;
#2414 = VECTOR('',#18715,1.) ;
#2415 = VECTOR('',#18716,1.) ;
#2416 = VECTOR('',#18719,1.) ;
#2417 = VECTOR('',#18720,1.) ;
#2418 = VECTOR('',#18721,1.) ;
#2419 = VECTOR('',#18726,1.) ;
#2420 = VECTOR('',#18733,1.) ;
#2421 = VECTOR('',#18734,1.) ;
#2422 = VECTOR('',#18735,1.) ;
#2423 = VECTOR('',#18738,1.) ;
#2424 = VECTOR('',#18739,1.) ;
#2425 = VECTOR('',#18740,1.) ;
#2426 = VECTOR('',#18743,1.) ;
#2427 = VECTOR('',#18744,1.) ;
#2428 = VECTOR('',#18745,1.) ;
#2429 = VECTOR('',#18750,1.) ;
#2430 = VECTOR('',#18757,1.) ;
#2431 = VECTOR('',#18758,1.) ;
#2432 = VECTOR('',#18759,1.) ;
#2433 = VECTOR('',#18762,1.) ;
#2434 = VECTOR('',#18763,1.) ;
#2435 = VECTOR('',#18764,1.) ;
#2436 = VECTOR('',#18767,1.) ;
#2437 = VECTOR('',#18768,1.) ;
#2438 = VECTOR('',#18769,1.) ;
#2439 = VECTOR('',#18774,1.) ;
#2440 = VECTOR('',#18781,1.) ;
#2441 = VECTOR('',#18782,1.) ;
#2442 = VECTOR('',#18783,1.) ;
#2443 = VECTOR('',#18788,1.) ;
#2444 = VECTOR('',#18789,1.) ;
#2445 = VECTOR('',#18790,1.) ;
#2446 = VECTOR('',#18793,1.) ;
#2447 = VECTOR('',#18794,1.) ;
#2448 = VECTOR('',#18795,1.) ;
#2449 = VECTOR('',#18800,1.) ;
#2450 = VECTOR('',#18809,1.) ;
#2451 = VECTOR('',#18810,1.) ;
#2452 = VECTOR('',#18811,1.) ;
#2453 = VECTOR('',#18814,1.) ;
#2454 = VECTOR('',#18815,1.) ;
#2455 = VECTOR('',#18816,1.) ;
#2456 = VECTOR('',#18819,1.) ;
#2457 = VECTOR('',#18820,1.) ;
#2458 = VECTOR('',#18821,1.) ;
#2459 = VECTOR('',#18826,1.) ;
#2460 = VECTOR('',#18833,1.) ;
#2461 = VECTOR('',#18834,1.) ;
#2462 = VECTOR('',#18835,1.) ;
#2463 = VECTOR('',#18838,1.) ;
#2464 = VECTOR('',#18839,1.) ;
#2465 = VECTOR('',#18840,1.) ;
#2466 = VECTOR('',#18843,1.) ;
#2467 = VECTOR('',#18844,1.) ;
#2468 = VECTOR('',#18845,1.) ;
#2469 = VECTOR('',#18850,1.) ;
#2470 = VECTOR('',#18857,1.) ;
#2471 = VECTOR('',#18858,1.) ;
#2472 = VECTOR('',#18859,1.) ;
#2473 = VECTOR('',#18862,1.) ;
#2474 = VECTOR('',#18863,1.) ;
#2475 = VECTOR('',#18864,1.) ;
#2476 = VECTOR('',#18867,1.) ;
#2477 = VECTOR('',#18868,1.) ;
#2478 = VECTOR('',#18869,1.) ;
#2479 = VECTOR('',#18874,1.) ;
#2480 = VECTOR('',#18881,1.) ;
#2481 = VECTOR('',#18882,1.) ;
#2482 = VECTOR('',#18883,1.) ;
#2483 = VECTOR('',#18886,1.) ;
#2484 = VECTOR('',#18887,1.) ;
#2485 = VECTOR('',#18888,1.) ;
#2486 = VECTOR('',#18891,1.) ;
#2487 = VECTOR('',#18892,1.) ;
#2488 = VECTOR('',#18893,1.) ;
#2489 = VECTOR('',#18898,1.) ;
#2490 = VECTOR('',#18905,1.) ;
#2491 = VECTOR('',#18906,1.) ;
#2492 = VECTOR('',#18907,1.) ;
#2493 = VECTOR('',#18910,1.) ;
#2494 = VECTOR('',#18911,1.) ;
#2495 = VECTOR('',#18912,1.) ;
#2496 = VECTOR('',#18915,1.) ;
#2497 = VECTOR('',#18916,1.) ;
#2498 = VECTOR('',#18917,1.) ;
#2499 = VECTOR('',#18922,1.) ;
#2500 = VECTOR('',#18929,1.5) ;
#2501 = VECTOR('',#18930,1.5) ;
#2502 = VECTOR('',#18943,1.) ;
#2503 = VECTOR('',#18950,1.29) ;
#2504 = VECTOR('',#18961,1.) ;
#2505 = VECTOR('',#18964,1.) ;
#2506 = VECTOR('',#18971,1.4) ;
#2507 = VECTOR('',#18976,1.) ;
#2508 = VECTOR('',#18977,1.) ;
#2509 = VECTOR('',#18978,1.23) ;
#2510 = VECTOR('',#18987,1.4) ;
#2511 = VECTOR('',#19028,1.4) ;
#2512 = VECTOR('',#19035,1.4) ;
#2513 = VECTOR('',#19040,1.31) ;
#2514 = VECTOR('',#19047,1.4) ;
#2515 = VECTOR('',#19054,1.) ;
#2516 = VECTOR('',#19055,1.) ;
#2517 = VECTOR('',#19056,1.) ;
#2518 = VECTOR('',#19057,1.) ;
#2519 = VECTOR('',#19060,1.) ;
#2520 = VECTOR('',#19061,1.) ;
#2521 = VECTOR('',#19062,1.) ;
#2522 = VECTOR('',#19063,1.) ;
#2523 = VECTOR('',#19066,1.) ;
#2524 = VECTOR('',#19067,1.) ;
#2525 = VECTOR('',#19068,1.) ;
#2526 = VECTOR('',#19069,1.) ;
#2527 = VECTOR('',#19072,1.) ;
#2528 = VECTOR('',#19073,1.) ;
#2529 = VECTOR('',#19094,1.) ;
#2530 = VECTOR('',#19095,1.) ;
#2531 = VECTOR('',#19096,1.) ;
#2532 = VECTOR('',#19097,1.) ;
#2533 = VECTOR('',#19100,1.) ;
#2534 = VECTOR('',#19101,1.) ;
#2535 = VECTOR('',#19102,1.) ;
#2536 = VECTOR('',#19103,1.) ;
#2537 = VECTOR('',#19106,1.) ;
#2538 = VECTOR('',#19107,1.) ;
#2539 = VECTOR('',#19108,1.) ;
#2540 = VECTOR('',#19109,1.) ;
#2541 = VECTOR('',#19112,1.) ;
#2542 = VECTOR('',#19113,1.) ;
#2543 = VECTOR('',#19160,1.1) ;
#2544 = VECTOR('',#19165,1.45) ;
#2545 = VECTOR('',#19166,1.45) ;
#2546 = VECTOR('',#19173,1.75) ;
#2547 = VECTOR('',#19174,1.75) ;
#2548 = VECTOR('',#19185,1.) ;
#2549 = VECTOR('',#19188,1.) ;
#2550 = VECTOR('',#19201,1.) ;
#2551 = VECTOR('',#19202,1.) ;
#2552 = VECTOR('',#19207,0.7) ;
#2553 = VECTOR('',#19208,0.7) ;
#2554 = VECTOR('',#19215,1.225) ;
#2555 = VECTOR('',#19222,1.) ;
#2556 = VECTOR('',#19223,1.) ;
#2557 = VECTOR('',#19228,1.225) ;
#2558 = VECTOR('',#19239,0.85) ;
#2559 = VECTOR('',#19246,1.09) ;
#2560 = VECTOR('',#19259,0.35) ;
#2561 = VECTOR('',#19266,0.35) ;
#2562 = VECTOR('',#19273,0.35) ;
#2563 = VECTOR('',#19280,0.35) ;
#2564 = VECTOR('',#19287,1.75) ;
#2565 = VECTOR('',#19294,3.5) ;
#2566 = VECTOR('',#19307,0.35) ;
#2567 = VECTOR('',#19314,0.35) ;
#2568 = VECTOR('',#19321,0.35) ;
#2569 = VECTOR('',#19328,0.35) ;
#2570 = VECTOR('',#19335,1.75) ;
#2571 = VECTOR('',#19342,3.5) ;
#2572 = VECTOR('',#19353,1.) ;
#2573 = VECTOR('',#19360,0.325) ;
#2574 = VECTOR('',#19367,1.) ;
#2575 = VECTOR('',#19374,0.325) ;
#2576 = VECTOR('',#19381,1.) ;
#2577 = VECTOR('',#19382,1.) ;
#2578 = VECTOR('',#19383,1.) ;
#2579 = VECTOR('',#19384,1.) ;
#2580 = VECTOR('',#19387,1.) ;
#2581 = VECTOR('',#19388,1.) ;
#2582 = VECTOR('',#19389,1.) ;
#2583 = VECTOR('',#19390,1.) ;
#2584 = VECTOR('',#19393,1.) ;
#2585 = VECTOR('',#19394,1.) ;
#2586 = VECTOR('',#19395,1.) ;
#2587 = VECTOR('',#19396,1.) ;
#2588 = VECTOR('',#19399,1.) ;
#2589 = VECTOR('',#19400,1.) ;
#2590 = VECTOR('',#19403,1.) ;
#2591 = VECTOR('',#19404,1.) ;
#2592 = VECTOR('',#19417,1.75) ;
#2593 = VECTOR('',#19444,0.195) ;
#2594 = VECTOR('',#19453,0.35) ;
#2595 = VECTOR('',#19466,0.525) ;
#2596 = VECTOR('',#19473,1.) ;
#2597 = VECTOR('',#19486,0.5) ;
#2598 = VECTOR('',#19491,1.) ;
#2599 = VECTOR('',#19492,1.) ;
#2600 = VECTOR('',#19493,1.) ;
#2601 = VECTOR('',#19494,1.) ;
#2602 = VECTOR('',#19497,1.) ;
#2603 = VECTOR('',#19498,1.) ;
#2604 = VECTOR('',#19499,1.) ;
#2605 = VECTOR('',#19500,1.) ;
#2606 = VECTOR('',#19503,1.) ;
#2607 = VECTOR('',#19504,1.) ;
#2608 = VECTOR('',#19505,1.) ;
#2609 = VECTOR('',#19506,1.) ;
#2610 = VECTOR('',#19509,1.) ;
#2611 = VECTOR('',#19510,1.) ;
#2612 = VECTOR('',#19513,1.) ;
#2613 = VECTOR('',#19514,1.) ;
#2614 = VECTOR('',#19517,1.) ;
#2615 = VECTOR('',#19520,1.) ;
#2616 = VECTOR('',#19529,0.4) ;
#2617 = VECTOR('',#19536,1.) ;
#2618 = VECTOR('',#19537,1.) ;
#2619 = VECTOR('',#19538,1.) ;
#2620 = VECTOR('',#19539,1.) ;
#2621 = VECTOR('',#19542,1.) ;
#2622 = VECTOR('',#19543,1.) ;
#2623 = VECTOR('',#19544,1.) ;
#2624 = VECTOR('',#19545,1.) ;
#2625 = VECTOR('',#19548,1.) ;
#2626 = VECTOR('',#19549,1.) ;
#2627 = VECTOR('',#19550,1.) ;
#2628 = VECTOR('',#19551,1.) ;
#2629 = VECTOR('',#19554,1.) ;
#2630 = VECTOR('',#19555,1.) ;
#2631 = VECTOR('',#19558,1.) ;
#2632 = VECTOR('',#19559,1.) ;
#2633 = VECTOR('',#19562,1.) ;
#2634 = VECTOR('',#19565,1.) ;
#2635 = VECTOR('',#19574,0.3) ;
#2636 = VECTOR('',#19581,1.) ;
#2637 = VECTOR('',#19582,1.) ;
#2638 = VECTOR('',#19583,1.) ;
#2639 = VECTOR('',#19584,1.) ;
#2640 = VECTOR('',#19587,1.) ;
#2641 = VECTOR('',#19588,1.) ;
#2642 = VECTOR('',#19589,1.) ;
#2643 = VECTOR('',#19590,1.) ;
#2644 = VECTOR('',#19593,1.) ;
#2645 = VECTOR('',#19594,1.) ;
#2646 = VECTOR('',#19595,1.) ;
#2647 = VECTOR('',#19596,1.) ;
#2648 = VECTOR('',#19599,1.) ;
#2649 = VECTOR('',#19600,1.) ;
#2650 = VECTOR('',#19603,1.) ;
#2651 = VECTOR('',#19604,1.) ;
#2652 = VECTOR('',#19607,1.) ;
#2653 = VECTOR('',#19610,1.) ;
#2654 = VECTOR('',#19619,0.3) ;
#2655 = VECTOR('',#19624,1.) ;
#2656 = VECTOR('',#19625,1.) ;
#2657 = VECTOR('',#19626,1.) ;
#2658 = VECTOR('',#19627,1.) ;
#2659 = VECTOR('',#19630,1.) ;
#2660 = VECTOR('',#19631,1.) ;
#2661 = VECTOR('',#19632,1.) ;
#2662 = VECTOR('',#19633,1.) ;
#2663 = VECTOR('',#19636,1.) ;
#2664 = VECTOR('',#19637,1.) ;
#2665 = VECTOR('',#19638,1.) ;
#2666 = VECTOR('',#19639,1.) ;
#2667 = VECTOR('',#19642,1.) ;
#2668 = VECTOR('',#19643,1.) ;
#2669 = VECTOR('',#19646,1.) ;
#2670 = VECTOR('',#19647,1.) ;
#2671 = VECTOR('',#19650,1.) ;
#2672 = VECTOR('',#19653,1.) ;
#2673 = CYLINDRICAL_SURFACE('',#13659,0.41) ;
#2674 = CYLINDRICAL_SURFACE('',#13662,11.4) ;
#2675 = CYLINDRICAL_SURFACE('',#13670,0.41) ;
#2676 = CYLINDRICAL_SURFACE('',#13680,0.325) ;
#2677 = CYLINDRICAL_SURFACE('',#13683,0.325) ;
#2678 = CYLINDRICAL_SURFACE('',#13686,0.325) ;
#2679 = CYLINDRICAL_SURFACE('',#13689,0.325) ;
#2680 = CYLINDRICAL_SURFACE('',#13692,0.325) ;
#2681 = CYLINDRICAL_SURFACE('',#13695,0.325) ;
#2682 = CYLINDRICAL_SURFACE('',#13707,12.5) ;
#2683 = CYLINDRICAL_SURFACE('',#13713,1.1) ;
#2684 = CYLINDRICAL_SURFACE('',#13716,1.5) ;
#2685 = CYLINDRICAL_SURFACE('',#13718,1.5) ;
#2686 = CYLINDRICAL_SURFACE('',#13724,0.9) ;
#2687 = CYLINDRICAL_SURFACE('',#13728,1.2) ;
#2688 = CYLINDRICAL_SURFACE('',#13735,1.5) ;
#2689 = CYLINDRICAL_SURFACE('',#13738,1.75) ;
#2690 = CYLINDRICAL_SURFACE('',#13742,1.75) ;
#2691 = CYLINDRICAL_SURFACE('',#13746,2.5) ;
#2692 = CYLINDRICAL_SURFACE('',#13749,2.5) ;
#2693 = CYLINDRICAL_SURFACE('',#13754,0.2025) ;
#2694 = CYLINDRICAL_SURFACE('',#13757,0.325) ;
#2695 = CYLINDRICAL_SURFACE('',#13760,0.325) ;
#2696 = CYLINDRICAL_SURFACE('',#13763,0.325) ;
#2697 = CYLINDRICAL_SURFACE('',#13766,0.325) ;
#2698 = CYLINDRICAL_SURFACE('',#13769,0.325) ;
#2699 = CYLINDRICAL_SURFACE('',#13772,0.325) ;
#2700 = CYLINDRICAL_SURFACE('',#13775,1.41) ;
#2701 = CYLINDRICAL_SURFACE('',#13778,1.8) ;
#2702 = CYLINDRICAL_SURFACE('',#13782,1.41) ;
#2703 = CYLINDRICAL_SURFACE('',#13785,1.8) ;
#2704 = CYLINDRICAL_SURFACE('',#13789,5.9) ;
#2705 = CYLINDRICAL_SURFACE('',#13794,5.5) ;
#2706 = CYLINDRICAL_SURFACE('',#13796,11.4) ;
#2707 = CYLINDRICAL_SURFACE('',#13800,12.5) ;
#2708 = CYLINDRICAL_SURFACE('',#13806,5.89) ;
#2709 = CYLINDRICAL_SURFACE('',#13812,0.325) ;
#2710 = CYLINDRICAL_SURFACE('',#13815,0.325) ;
#2711 = CYLINDRICAL_SURFACE('',#13818,0.325) ;
#2712 = CYLINDRICAL_SURFACE('',#13821,0.325) ;
#2713 = CYLINDRICAL_SURFACE('',#13824,0.325) ;
#2714 = CYLINDRICAL_SURFACE('',#13827,0.325) ;
#2715 = CYLINDRICAL_SURFACE('',#13830,11.4) ;
#2716 = CYLINDRICAL_SURFACE('',#13833,12.5) ;
#2717 = CYLINDRICAL_SURFACE('',#13844,0.75) ;
#2718 = CYLINDRICAL_SURFACE('',#13848,0.7) ;
#2719 = CYLINDRICAL_SURFACE('',#13854,0.75) ;
#2720 = CYLINDRICAL_SURFACE('',#13856,0.195) ;
#2721 = CYLINDRICAL_SURFACE('',#13859,0.195) ;
#2722 = CYLINDRICAL_SURFACE('',#13862,0.195) ;
#2723 = CYLINDRICAL_SURFACE('',#13867,2.5) ;
#2724 = CYLINDRICAL_SURFACE('',#13869,0.5) ;
#2725 = CYLINDRICAL_SURFACE('',#13876,0.15) ;
#2726 = CYLINDRICAL_SURFACE('',#13880,0.15) ;
#2727 = CYLINDRICAL_SURFACE('',#13884,0.15) ;
#2728 = CYLINDRICAL_SURFACE('',#13888,0.15) ;
#2729 = CYLINDRICAL_SURFACE('',#13892,0.15) ;
#2730 = CYLINDRICAL_SURFACE('',#13896,0.15) ;
#2731 = CYLINDRICAL_SURFACE('',#13900,0.15) ;
#2732 = CYLINDRICAL_SURFACE('',#13904,0.15) ;
#2733 = CYLINDRICAL_SURFACE('',#13908,0.15) ;
#2734 = CYLINDRICAL_SURFACE('',#13912,0.15) ;
#2735 = CYLINDRICAL_SURFACE('',#13916,0.15) ;
#2736 = CYLINDRICAL_SURFACE('',#13920,0.15) ;
#2737 = CYLINDRICAL_SURFACE('',#13924,0.15) ;
#2738 = CYLINDRICAL_SURFACE('',#13928,0.15) ;
#2739 = CYLINDRICAL_SURFACE('',#13932,0.15) ;
#2740 = CYLINDRICAL_SURFACE('',#13936,0.15) ;
#2741 = CYLINDRICAL_SURFACE('',#13940,0.15) ;
#2742 = CYLINDRICAL_SURFACE('',#13944,0.15) ;
#2743 = CYLINDRICAL_SURFACE('',#13948,0.15) ;
#2744 = CYLINDRICAL_SURFACE('',#13952,0.15) ;
#2745 = CYLINDRICAL_SURFACE('',#13956,0.15) ;
#2746 = CYLINDRICAL_SURFACE('',#13960,0.15) ;
#2747 = CYLINDRICAL_SURFACE('',#13964,0.15) ;
#2748 = CYLINDRICAL_SURFACE('',#13968,0.15) ;
#2749 = CYLINDRICAL_SURFACE('',#13972,0.4) ;
#2750 = CYLINDRICAL_SURFACE('',#13975,0.4) ;
#2751 = CYLINDRICAL_SURFACE('',#13978,0.4) ;
#2752 = CYLINDRICAL_SURFACE('',#13981,0.4) ;
#2753 = CYLINDRICAL_SURFACE('',#13984,0.4) ;
#2754 = CYLINDRICAL_SURFACE('',#13987,0.4) ;
#2755 = CYLINDRICAL_SURFACE('',#13990,0.4) ;
#2756 = CYLINDRICAL_SURFACE('',#13993,0.4) ;
#2757 = CYLINDRICAL_SURFACE('',#13996,0.4) ;
#2758 = CYLINDRICAL_SURFACE('',#13999,0.4) ;
#2759 = CYLINDRICAL_SURFACE('',#14002,0.4) ;
#2760 = CYLINDRICAL_SURFACE('',#14005,0.4) ;
#2761 = CYLINDRICAL_SURFACE('',#14008,0.4) ;
#2762 = CYLINDRICAL_SURFACE('',#14011,0.4) ;
#2763 = CYLINDRICAL_SURFACE('',#14014,0.4) ;
#2764 = CYLINDRICAL_SURFACE('',#14017,0.4) ;
#2765 = CYLINDRICAL_SURFACE('',#14020,0.4) ;
#2766 = CYLINDRICAL_SURFACE('',#14023,0.4) ;
#2767 = CYLINDRICAL_SURFACE('',#14026,0.4) ;
#2768 = CYLINDRICAL_SURFACE('',#14029,0.4) ;
#2769 = CYLINDRICAL_SURFACE('',#14032,0.4) ;
#2770 = CYLINDRICAL_SURFACE('',#14035,0.4) ;
#2771 = CYLINDRICAL_SURFACE('',#14038,0.4) ;
#2772 = CYLINDRICAL_SURFACE('',#14041,0.4) ;
#2773 = CYLINDRICAL_SURFACE('',#14044,0.215) ;
#2774 = CYLINDRICAL_SURFACE('',#14047,0.215) ;
#2775 = CYLINDRICAL_SURFACE('',#14050,0.215) ;
#2776 = CYLINDRICAL_SURFACE('',#14053,0.51) ;
#2777 = CYLINDRICAL_SURFACE('',#14056,10.) ;
#2778 = CYLINDRICAL_SURFACE('',#14068,1.05) ;
#2779 = CYLINDRICAL_SURFACE('',#14069,1.45) ;
#2780 = CYLINDRICAL_SURFACE('',#14073,1.75) ;
#2781 = CYLINDRICAL_SURFACE('',#14077,0.75) ;
#2782 = CYLINDRICAL_SURFACE('',#14085,1.05) ;
#2783 = CYLINDRICAL_SURFACE('',#14086,1.45) ;
#2784 = CYLINDRICAL_SURFACE('',#14090,1.75) ;
#2785 = CYLINDRICAL_SURFACE('',#14094,0.75) ;
#2786 = CYLINDRICAL_SURFACE('',#14096,0.75) ;
#2787 = CYLINDRICAL_SURFACE('',#14099,1.1) ;
#2788 = CYLINDRICAL_SURFACE('',#14110,0.705) ;
#2789 = CYLINDRICAL_SURFACE('',#14112,0.95) ;
#2790 = CYLINDRICAL_SURFACE('',#14122,0.75) ;
#2791 = CYLINDRICAL_SURFACE('',#14127,2.5) ;
#2792 = CYLINDRICAL_SURFACE('',#14130,2.5) ;
#2793 = CYLINDRICAL_SURFACE('',#14147,2.5) ;
#2794 = CYLINDRICAL_SURFACE('',#14152,2.5) ;
#2795 = CYLINDRICAL_SURFACE('',#14157,2.5) ;
#2796 = CYLINDRICAL_SURFACE('',#14162,2.5) ;
#2797 = CYLINDRICAL_SURFACE('',#14167,2.5) ;
#2798 = CYLINDRICAL_SURFACE('',#14172,2.5) ;
#2799 = CYLINDRICAL_SURFACE('',#14177,2.5) ;
#2800 = CYLINDRICAL_SURFACE('',#14182,2.5) ;
#2801 = CYLINDRICAL_SURFACE('',#14187,2.5) ;
#2802 = CYLINDRICAL_SURFACE('',#14192,2.5) ;
#2803 = CYLINDRICAL_SURFACE('',#14197,1.4) ;
#2804 = CYLINDRICAL_SURFACE('',#14208,10.2) ;
#2805 = CYLINDRICAL_SURFACE('',#14211,11.1) ;
#2806 = CYLINDRICAL_SURFACE('',#14228,0.25) ;
#2807 = CYLINDRICAL_SURFACE('',#14232,0.21) ;
#2808 = CYLINDRICAL_SURFACE('',#14235,0.5) ;
#2809 = CYLINDRICAL_SURFACE('',#14238,0.5) ;
#2810 = CYLINDRICAL_SURFACE('',#14241,0.5) ;
#2811 = CYLINDRICAL_SURFACE('',#14254,0.2) ;
#2812 = CYLINDRICAL_SURFACE('',#14401,0.05) ;
#2813 = CYLINDRICAL_SURFACE('',#14407,0.05) ;
#2814 = CYLINDRICAL_SURFACE('',#14410,0.05) ;
#2815 = CYLINDRICAL_SURFACE('',#14412,0.05) ;
#2816 = CYLINDRICAL_SURFACE('',#14414,0.05) ;
#2817 = CYLINDRICAL_SURFACE('',#14416,0.05) ;
#2818 = CYLINDRICAL_SURFACE('',#14419,0.05) ;
#2819 = CYLINDRICAL_SURFACE('',#14423,0.05) ;
#2820 = CYLINDRICAL_SURFACE('',#14426,0.05) ;
#2821 = CYLINDRICAL_SURFACE('',#14430,0.05) ;
#2822 = CYLINDRICAL_SURFACE('',#14433,0.05) ;
#2823 = CYLINDRICAL_SURFACE('',#14435,0.05) ;
#2824 = CYLINDRICAL_SURFACE('',#14437,0.05) ;
#2825 = CYLINDRICAL_SURFACE('',#14439,0.05) ;
#2826 = CYLINDRICAL_SURFACE('',#14442,0.05) ;
#2827 = CYLINDRICAL_SURFACE('',#14446,0.05) ;
#2828 = CYLINDRICAL_SURFACE('',#14449,0.05) ;
#2829 = CYLINDRICAL_SURFACE('',#14453,0.05) ;
#2830 = CYLINDRICAL_SURFACE('',#14456,0.05) ;
#2831 = CYLINDRICAL_SURFACE('',#14458,0.05) ;
#2832 = CYLINDRICAL_SURFACE('',#14460,0.05) ;
#2833 = CYLINDRICAL_SURFACE('',#14462,0.05) ;
#2834 = CYLINDRICAL_SURFACE('',#14465,0.05) ;
#2835 = CYLINDRICAL_SURFACE('',#14469,0.05) ;
#2836 = CYLINDRICAL_SURFACE('',#14472,0.05) ;
#2837 = CYLINDRICAL_SURFACE('',#14476,0.05) ;
#2838 = CYLINDRICAL_SURFACE('',#14479,0.05) ;
#2839 = CYLINDRICAL_SURFACE('',#14481,0.05) ;
#2840 = CYLINDRICAL_SURFACE('',#14483,0.05) ;
#2841 = CYLINDRICAL_SURFACE('',#14485,0.05) ;
#2842 = CYLINDRICAL_SURFACE('',#14488,0.05) ;
#2843 = CYLINDRICAL_SURFACE('',#14492,0.05) ;
#2844 = CYLINDRICAL_SURFACE('',#14508,1.1) ;
#2845 = CYLINDRICAL_SURFACE('',#14519,1.4) ;
#2846 = CYLINDRICAL_SURFACE('',#14630,1.1) ;
#2847 = CYLINDRICAL_SURFACE('',#14649,1.4) ;
#2848 = CYLINDRICAL_SURFACE('',#14689,1.1) ;
#2849 = CYLINDRICAL_SURFACE('',#14691,1.4) ;
#2850 = CYLINDRICAL_SURFACE('',#14699,1.4) ;
#2851 = CYLINDRICAL_SURFACE('',#14704,1.4) ;
#2852 = CYLINDRICAL_SURFACE('',#14706,1.4) ;
#2853 = CYLINDRICAL_SURFACE('',#14710,1.4) ;
#2854 = CYLINDRICAL_SURFACE('',#14712,1.4) ;
#2855 = CYLINDRICAL_SURFACE('',#14716,1.4) ;
#2856 = CYLINDRICAL_SURFACE('',#14722,1.4) ;
#2857 = CYLINDRICAL_SURFACE('',#14726,1.4) ;
#2858 = CYLINDRICAL_SURFACE('',#14728,1.4) ;
#2859 = CYLINDRICAL_SURFACE('',#14732,1.4) ;
#2860 = CYLINDRICAL_SURFACE('',#14738,1.4) ;
#2861 = CYLINDRICAL_SURFACE('',#14742,1.4) ;
#2862 = CYLINDRICAL_SURFACE('',#14744,1.4) ;
#2863 = CYLINDRICAL_SURFACE('',#14748,1.4) ;
#2864 = CYLINDRICAL_SURFACE('',#14754,1.4) ;
#2865 = CYLINDRICAL_SURFACE('',#14759,1.4) ;
#2866 = CYLINDRICAL_SURFACE('',#14760,1.4) ;
#2867 = CYLINDRICAL_SURFACE('',#14771,1.1) ;
#2868 = CYLINDRICAL_SURFACE('',#14803,0.45) ;
#2869 = CYLINDRICAL_SURFACE('',#14807,0.45) ;
#2870 = CYLINDRICAL_SURFACE('',#14811,0.425) ;
#2871 = CYLINDRICAL_SURFACE('',#14814,0.45) ;
#2872 = CYLINDRICAL_SURFACE('',#14818,0.45) ;
#2873 = CYLINDRICAL_SURFACE('',#14822,0.425) ;
#2874 = CYLINDRICAL_SURFACE('',#14864,0.7) ;
#2875 = CYLINDRICAL_SURFACE('',#14916,1.3) ;
#2876 = CYLINDRICAL_SURFACE('',#14918,0.6) ;
#2877 = CYLINDRICAL_SURFACE('',#14921,0.6) ;
#2878 = CYLINDRICAL_SURFACE('',#14924,1.6) ;
#2879 = CYLINDRICAL_SURFACE('',#14931,1.8) ;
#2880 = CYLINDRICAL_SURFACE('',#14940,0.4) ;
#2881 = CYLINDRICAL_SURFACE('',#14943,0.3) ;
#2882 = CYLINDRICAL_SURFACE('',#14962,1.5) ;
#2883 = CYLINDRICAL_SURFACE('',#14964,0.3) ;
#2884 = CYLINDRICAL_SURFACE('',#14966,1.5) ;
#2885 = CYLINDRICAL_SURFACE('',#14968,0.3) ;
#2886 = CYLINDRICAL_SURFACE('',#14970,1.5) ;
#2887 = CYLINDRICAL_SURFACE('',#14972,0.3) ;
#2888 = CYLINDRICAL_SURFACE('',#14974,1.5) ;
#2889 = CYLINDRICAL_SURFACE('',#14976,0.3) ;
#2890 = CYLINDRICAL_SURFACE('',#14978,1.5) ;
#2891 = CYLINDRICAL_SURFACE('',#14980,0.3) ;
#2892 = CYLINDRICAL_SURFACE('',#14982,1.5) ;
#2893 = CYLINDRICAL_SURFACE('',#14984,0.3) ;
#2894 = CYLINDRICAL_SURFACE('',#14986,1.5) ;
#2895 = CYLINDRICAL_SURFACE('',#14988,0.3) ;
#2896 = CYLINDRICAL_SURFACE('',#14992,1.5) ;
#2897 = CYLINDRICAL_SURFACE('',#14994,0.4) ;
#2898 = CYLINDRICAL_SURFACE('',#15000,0.4) ;
#2899 = CYLINDRICAL_SURFACE('',#15003,0.6) ;
#2900 = CYLINDRICAL_SURFACE('',#15009,0.4) ;
#2901 = CYLINDRICAL_SURFACE('',#15012,0.8) ;
#2902 = CYLINDRICAL_SURFACE('',#15088,1.5) ;
#2903 = CYLINDRICAL_SURFACE('',#15094,1.) ;
#2904 = CYLINDRICAL_SURFACE('',#15097,1.29) ;
#2905 = CYLINDRICAL_SURFACE('',#15106,1.4) ;
#2906 = CYLINDRICAL_SURFACE('',#15109,1.23) ;
#2907 = CYLINDRICAL_SURFACE('',#15112,1.4) ;
#2908 = CYLINDRICAL_SURFACE('',#15117,1.4) ;
#2909 = CYLINDRICAL_SURFACE('',#15133,1.4) ;
#2910 = CYLINDRICAL_SURFACE('',#15136,1.4) ;
#2911 = CYLINDRICAL_SURFACE('',#15138,1.31) ;
#2912 = CYLINDRICAL_SURFACE('',#15140,1.4) ;
#2913 = CYLINDRICAL_SURFACE('',#15151,1.41) ;
#2914 = CYLINDRICAL_SURFACE('',#15153,1.75) ;
#2915 = CYLINDRICAL_SURFACE('',#15161,1.75) ;
#2916 = CYLINDRICAL_SURFACE('',#15164,1.41) ;
#2917 = CYLINDRICAL_SURFACE('',#15183,1.1) ;
#2918 = CYLINDRICAL_SURFACE('',#15184,1.45) ;
#2919 = CYLINDRICAL_SURFACE('',#15187,1.75) ;
#2920 = CYLINDRICAL_SURFACE('',#15196,1.1) ;
#2921 = CYLINDRICAL_SURFACE('',#15198,1.1) ;
#2922 = CYLINDRICAL_SURFACE('',#15201,0.7) ;
#2923 = CYLINDRICAL_SURFACE('',#15208,1.) ;
#2924 = CYLINDRICAL_SURFACE('',#15214,0.85) ;
#2925 = CYLINDRICAL_SURFACE('',#15217,1.09) ;
#2926 = CYLINDRICAL_SURFACE('',#15223,0.35) ;
#2927 = CYLINDRICAL_SURFACE('',#15226,0.35) ;
#2928 = CYLINDRICAL_SURFACE('',#15229,0.35) ;
#2929 = CYLINDRICAL_SURFACE('',#15232,0.35) ;
#2930 = CYLINDRICAL_SURFACE('',#15235,1.75) ;
#2931 = CYLINDRICAL_SURFACE('',#15238,3.5) ;
#2932 = CYLINDRICAL_SURFACE('',#15244,0.35) ;
#2933 = CYLINDRICAL_SURFACE('',#15247,0.35) ;
#2934 = CYLINDRICAL_SURFACE('',#15250,0.35) ;
#2935 = CYLINDRICAL_SURFACE('',#15253,0.35) ;
#2936 = CYLINDRICAL_SURFACE('',#15256,1.75) ;
#2937 = CYLINDRICAL_SURFACE('',#15259,3.5) ;
#2938 = CYLINDRICAL_SURFACE('',#15267,0.325) ;
#2939 = CYLINDRICAL_SURFACE('',#15270,0.325) ;
#2940 = CYLINDRICAL_SURFACE('',#15273,0.325) ;
#2941 = CYLINDRICAL_SURFACE('',#15276,0.325) ;
#2942 = CYLINDRICAL_SURFACE('',#15285,2.05) ;
#2943 = CYLINDRICAL_SURFACE('',#15287,1.75) ;
#2944 = CYLINDRICAL_SURFACE('',#15299,0.195) ;
#2945 = CYLINDRICAL_SURFACE('',#15303,0.35) ;
#2946 = CYLINDRICAL_SURFACE('',#15309,0.525) ;
#2947 = CYLINDRICAL_SURFACE('',#15312,1.) ;
#2948 = CYLINDRICAL_SURFACE('',#15318,0.5) ;
#2949 = CYLINDRICAL_SURFACE('',#15330,0.4) ;
#2950 = CYLINDRICAL_SURFACE('',#15343,0.3) ;
#2951 = CYLINDRICAL_SURFACE('',#15356,0.3) ;
#2952 = FACE_OUTER_BOUND('',#3719,.T.) ;
#2953 = FACE_OUTER_BOUND('',#3720,.T.) ;
#2954 = FACE_OUTER_BOUND('',#3721,.T.) ;
#2955 = FACE_OUTER_BOUND('',#3723,.T.) ;
#2956 = FACE_OUTER_BOUND('',#3724,.T.) ;
#2957 = FACE_OUTER_BOUND('',#3725,.T.) ;
#2958 = FACE_OUTER_BOUND('',#3727,.T.) ;
#2959 = FACE_OUTER_BOUND('',#3728,.T.) ;
#2960 = FACE_OUTER_BOUND('',#3729,.T.) ;
#2961 = FACE_OUTER_BOUND('',#3730,.T.) ;
#2962 = FACE_OUTER_BOUND('',#3731,.T.) ;
#2963 = FACE_OUTER_BOUND('',#3732,.T.) ;
#2964 = FACE_OUTER_BOUND('',#3733,.T.) ;
#2965 = FACE_OUTER_BOUND('',#3734,.T.) ;
#2966 = FACE_OUTER_BOUND('',#3735,.T.) ;
#2967 = FACE_OUTER_BOUND('',#3736,.T.) ;
#2968 = FACE_OUTER_BOUND('',#3737,.T.) ;
#2969 = FACE_OUTER_BOUND('',#3740,.T.) ;
#2970 = FACE_OUTER_BOUND('',#3741,.T.) ;
#2971 = FACE_OUTER_BOUND('',#3742,.T.) ;
#2972 = FACE_OUTER_BOUND('',#3744,.T.) ;
#2973 = FACE_OUTER_BOUND('',#3745,.T.) ;
#2974 = FACE_OUTER_BOUND('',#3746,.T.) ;
#2975 = FACE_OUTER_BOUND('',#3747,.T.) ;
#2976 = FACE_OUTER_BOUND('',#3749,.T.) ;
#2977 = FACE_OUTER_BOUND('',#3750,.T.) ;
#2978 = FACE_OUTER_BOUND('',#3751,.T.) ;
#2979 = FACE_OUTER_BOUND('',#3752,.T.) ;
#2980 = FACE_OUTER_BOUND('',#3753,.T.) ;
#2981 = FACE_OUTER_BOUND('',#3754,.T.) ;
#2982 = FACE_OUTER_BOUND('',#3756,.T.) ;
#2983 = FACE_OUTER_BOUND('',#3764,.T.) ;
#2984 = FACE_OUTER_BOUND('',#3765,.T.) ;
#2985 = FACE_OUTER_BOUND('',#3766,.T.) ;
#2986 = FACE_OUTER_BOUND('',#3768,.T.) ;
#2987 = FACE_OUTER_BOUND('',#3769,.T.) ;
#2988 = FACE_OUTER_BOUND('',#3771,.T.) ;
#2989 = FACE_OUTER_BOUND('',#3772,.T.) ;
#2990 = FACE_OUTER_BOUND('',#3774,.T.) ;
#2991 = FACE_OUTER_BOUND('',#3775,.T.) ;
#2992 = FACE_OUTER_BOUND('',#3777,.T.) ;
#2993 = FACE_OUTER_BOUND('',#3785,.T.) ;
#2994 = FACE_OUTER_BOUND('',#3786,.T.) ;
#2995 = FACE_OUTER_BOUND('',#3787,.T.) ;
#2996 = FACE_OUTER_BOUND('',#3788,.T.) ;
#2997 = FACE_OUTER_BOUND('',#3789,.T.) ;
#2998 = FACE_OUTER_BOUND('',#3790,.T.) ;
#2999 = FACE_OUTER_BOUND('',#3791,.T.) ;
#3000 = FACE_OUTER_BOUND('',#3792,.T.) ;
#3001 = FACE_OUTER_BOUND('',#3793,.T.) ;
#3002 = FACE_OUTER_BOUND('',#3794,.T.) ;
#3003 = FACE_OUTER_BOUND('',#3796,.T.) ;
#3004 = FACE_OUTER_BOUND('',#3797,.T.) ;
#3005 = FACE_OUTER_BOUND('',#3798,.T.) ;
#3006 = FACE_OUTER_BOUND('',#3800,.T.) ;
#3007 = FACE_OUTER_BOUND('',#3801,.T.) ;
#3008 = FACE_OUTER_BOUND('',#3803,.T.) ;
#3009 = FACE_OUTER_BOUND('',#3804,.T.) ;
#3010 = FACE_OUTER_BOUND('',#3805,.T.) ;
#3011 = FACE_OUTER_BOUND('',#3810,.T.) ;
#3012 = FACE_OUTER_BOUND('',#3811,.T.) ;
#3013 = FACE_OUTER_BOUND('',#3819,.T.) ;
#3014 = FACE_OUTER_BOUND('',#3830,.T.) ;
#3015 = FACE_OUTER_BOUND('',#3831,.T.) ;
#3016 = FACE_OUTER_BOUND('',#3832,.T.) ;
#3017 = FACE_OUTER_BOUND('',#3833,.T.) ;
#3018 = FACE_OUTER_BOUND('',#3834,.T.) ;
#3019 = FACE_OUTER_BOUND('',#3835,.T.) ;
#3020 = FACE_OUTER_BOUND('',#3836,.T.) ;
#3021 = FACE_OUTER_BOUND('',#3837,.T.) ;
#3022 = FACE_OUTER_BOUND('',#3838,.T.) ;
#3023 = FACE_OUTER_BOUND('',#3839,.T.) ;
#3024 = FACE_OUTER_BOUND('',#3840,.T.) ;
#3025 = FACE_OUTER_BOUND('',#3841,.T.) ;
#3026 = FACE_OUTER_BOUND('',#3849,.T.) ;
#3027 = FACE_OUTER_BOUND('',#3857,.T.) ;
#3028 = FACE_OUTER_BOUND('',#3858,.T.) ;
#3029 = FACE_OUTER_BOUND('',#3859,.T.) ;
#3030 = FACE_OUTER_BOUND('',#3860,.T.) ;
#3031 = FACE_OUTER_BOUND('',#3861,.T.) ;
#3032 = FACE_OUTER_BOUND('',#3862,.T.) ;
#3033 = FACE_OUTER_BOUND('',#3863,.T.) ;
#3034 = FACE_OUTER_BOUND('',#3865,.T.) ;
#3035 = FACE_OUTER_BOUND('',#3867,.T.) ;
#3036 = FACE_OUTER_BOUND('',#3868,.T.) ;
#3037 = FACE_OUTER_BOUND('',#3869,.T.) ;
#3038 = FACE_OUTER_BOUND('',#3870,.T.) ;
#3039 = FACE_OUTER_BOUND('',#3871,.T.) ;
#3040 = FACE_OUTER_BOUND('',#3876,.T.) ;
#3041 = FACE_OUTER_BOUND('',#3877,.T.) ;
#3042 = FACE_OUTER_BOUND('',#3878,.T.) ;
#3043 = FACE_OUTER_BOUND('',#3879,.T.) ;
#3044 = FACE_OUTER_BOUND('',#3880,.T.) ;
#3045 = FACE_OUTER_BOUND('',#3885,.T.) ;
#3046 = FACE_OUTER_BOUND('',#3886,.T.) ;
#3047 = FACE_OUTER_BOUND('',#3887,.T.) ;
#3048 = FACE_OUTER_BOUND('',#3888,.T.) ;
#3049 = FACE_OUTER_BOUND('',#3889,.T.) ;
#3050 = FACE_OUTER_BOUND('',#3890,.T.) ;
#3051 = FACE_OUTER_BOUND('',#3891,.T.) ;
#3052 = FACE_OUTER_BOUND('',#3892,.T.) ;
#3053 = FACE_OUTER_BOUND('',#3893,.T.) ;
#3054 = FACE_OUTER_BOUND('',#3894,.T.) ;
#3055 = FACE_OUTER_BOUND('',#3895,.T.) ;
#3056 = FACE_OUTER_BOUND('',#3896,.T.) ;
#3057 = FACE_OUTER_BOUND('',#3897,.T.) ;
#3058 = FACE_OUTER_BOUND('',#3898,.T.) ;
#3059 = FACE_OUTER_BOUND('',#3899,.T.) ;
#3060 = FACE_OUTER_BOUND('',#3900,.T.) ;
#3061 = FACE_OUTER_BOUND('',#3901,.T.) ;
#3062 = FACE_OUTER_BOUND('',#3902,.T.) ;
#3063 = FACE_OUTER_BOUND('',#3903,.T.) ;
#3064 = FACE_OUTER_BOUND('',#3904,.T.) ;
#3065 = FACE_OUTER_BOUND('',#3905,.T.) ;
#3066 = FACE_OUTER_BOUND('',#3906,.T.) ;
#3067 = FACE_OUTER_BOUND('',#3907,.T.) ;
#3068 = FACE_OUTER_BOUND('',#3908,.T.) ;
#3069 = FACE_OUTER_BOUND('',#3909,.T.) ;
#3070 = FACE_OUTER_BOUND('',#3910,.T.) ;
#3071 = FACE_OUTER_BOUND('',#3911,.T.) ;
#3072 = FACE_OUTER_BOUND('',#3912,.T.) ;
#3073 = FACE_OUTER_BOUND('',#3913,.T.) ;
#3074 = FACE_OUTER_BOUND('',#3914,.T.) ;
#3075 = FACE_OUTER_BOUND('',#3915,.T.) ;
#3076 = FACE_OUTER_BOUND('',#3916,.T.) ;
#3077 = FACE_OUTER_BOUND('',#3917,.T.) ;
#3078 = FACE_OUTER_BOUND('',#3918,.T.) ;
#3079 = FACE_OUTER_BOUND('',#3919,.T.) ;
#3080 = FACE_OUTER_BOUND('',#3920,.T.) ;
#3081 = FACE_OUTER_BOUND('',#3921,.T.) ;
#3082 = FACE_OUTER_BOUND('',#3922,.T.) ;
#3083 = FACE_OUTER_BOUND('',#3923,.T.) ;
#3084 = FACE_OUTER_BOUND('',#3924,.T.) ;
#3085 = FACE_OUTER_BOUND('',#3925,.T.) ;
#3086 = FACE_OUTER_BOUND('',#3926,.T.) ;
#3087 = FACE_OUTER_BOUND('',#3927,.T.) ;
#3088 = FACE_OUTER_BOUND('',#3928,.T.) ;
#3089 = FACE_OUTER_BOUND('',#3929,.T.) ;
#3090 = FACE_OUTER_BOUND('',#3930,.T.) ;
#3091 = FACE_OUTER_BOUND('',#3931,.T.) ;
#3092 = FACE_OUTER_BOUND('',#3932,.T.) ;
#3093 = FACE_OUTER_BOUND('',#3933,.T.) ;
#3094 = FACE_OUTER_BOUND('',#3934,.T.) ;
#3095 = FACE_OUTER_BOUND('',#3935,.T.) ;
#3096 = FACE_OUTER_BOUND('',#3936,.T.) ;
#3097 = FACE_OUTER_BOUND('',#3937,.T.) ;
#3098 = FACE_OUTER_BOUND('',#3938,.T.) ;
#3099 = FACE_OUTER_BOUND('',#3939,.T.) ;
#3100 = FACE_OUTER_BOUND('',#3940,.T.) ;
#3101 = FACE_OUTER_BOUND('',#3941,.T.) ;
#3102 = FACE_OUTER_BOUND('',#3942,.T.) ;
#3103 = FACE_OUTER_BOUND('',#3943,.T.) ;
#3104 = FACE_OUTER_BOUND('',#3944,.T.) ;
#3105 = FACE_OUTER_BOUND('',#3945,.T.) ;
#3106 = FACE_OUTER_BOUND('',#3946,.T.) ;
#3107 = FACE_OUTER_BOUND('',#3947,.T.) ;
#3108 = FACE_OUTER_BOUND('',#3948,.T.) ;
#3109 = FACE_OUTER_BOUND('',#3949,.T.) ;
#3110 = FACE_OUTER_BOUND('',#3950,.T.) ;
#3111 = FACE_OUTER_BOUND('',#3951,.T.) ;
#3112 = FACE_OUTER_BOUND('',#3952,.T.) ;
#3113 = FACE_OUTER_BOUND('',#3953,.T.) ;
#3114 = FACE_OUTER_BOUND('',#3954,.T.) ;
#3115 = FACE_OUTER_BOUND('',#3955,.T.) ;
#3116 = FACE_OUTER_BOUND('',#3956,.T.) ;
#3117 = FACE_OUTER_BOUND('',#3957,.T.) ;
#3118 = FACE_OUTER_BOUND('',#3958,.T.) ;
#3119 = FACE_OUTER_BOUND('',#3959,.T.) ;
#3120 = FACE_OUTER_BOUND('',#3960,.T.) ;
#3121 = FACE_OUTER_BOUND('',#3961,.T.) ;
#3122 = FACE_OUTER_BOUND('',#3962,.T.) ;
#3123 = FACE_OUTER_BOUND('',#4015,.T.) ;
#3124 = FACE_OUTER_BOUND('',#4044,.T.) ;
#3125 = FACE_OUTER_BOUND('',#4046,.T.) ;
#3126 = FACE_OUTER_BOUND('',#4048,.T.) ;
#3127 = FACE_OUTER_BOUND('',#4049,.T.) ;
#3128 = FACE_OUTER_BOUND('',#4050,.T.) ;
#3129 = FACE_OUTER_BOUND('',#4052,.T.) ;
#3130 = FACE_OUTER_BOUND('',#4053,.T.) ;
#3131 = FACE_OUTER_BOUND('',#4055,.T.) ;
#3132 = FACE_OUTER_BOUND('',#4056,.T.) ;
#3133 = FACE_OUTER_BOUND('',#4058,.T.) ;
#3134 = FACE_OUTER_BOUND('',#4060,.T.) ;
#3135 = FACE_OUTER_BOUND('',#4061,.T.) ;
#3136 = FACE_OUTER_BOUND('',#4062,.T.) ;
#3137 = FACE_OUTER_BOUND('',#4064,.T.) ;
#3138 = FACE_OUTER_BOUND('',#4065,.T.) ;
#3139 = FACE_OUTER_BOUND('',#4067,.T.) ;
#3140 = FACE_OUTER_BOUND('',#4068,.T.) ;
#3141 = FACE_OUTER_BOUND('',#4069,.T.) ;
#3142 = FACE_OUTER_BOUND('',#4070,.T.) ;
#3143 = FACE_OUTER_BOUND('',#4072,.T.) ;
#3144 = FACE_OUTER_BOUND('',#4074,.T.) ;
#3145 = FACE_OUTER_BOUND('',#4075,.T.) ;
#3146 = FACE_OUTER_BOUND('',#4076,.T.) ;
#3147 = FACE_OUTER_BOUND('',#4077,.T.) ;
#3148 = FACE_OUTER_BOUND('',#4078,.T.) ;
#3149 = FACE_OUTER_BOUND('',#4079,.T.) ;
#3150 = FACE_OUTER_BOUND('',#4080,.T.) ;
#3151 = FACE_OUTER_BOUND('',#4081,.T.) ;
#3152 = FACE_OUTER_BOUND('',#4082,.T.) ;
#3153 = FACE_OUTER_BOUND('',#4083,.T.) ;
#3154 = FACE_OUTER_BOUND('',#4085,.T.) ;
#3155 = FACE_OUTER_BOUND('',#4086,.T.) ;
#3156 = FACE_OUTER_BOUND('',#4087,.T.) ;
#3157 = FACE_OUTER_BOUND('',#4088,.T.) ;
#3158 = FACE_OUTER_BOUND('',#4089,.T.) ;
#3159 = FACE_OUTER_BOUND('',#4090,.T.) ;
#3160 = FACE_OUTER_BOUND('',#4091,.T.) ;
#3161 = FACE_OUTER_BOUND('',#4093,.T.) ;
#3162 = FACE_OUTER_BOUND('',#4094,.T.) ;
#3163 = FACE_OUTER_BOUND('',#4095,.T.) ;
#3164 = FACE_OUTER_BOUND('',#4096,.T.) ;
#3165 = FACE_OUTER_BOUND('',#4097,.T.) ;
#3166 = FACE_OUTER_BOUND('',#4098,.T.) ;
#3167 = FACE_OUTER_BOUND('',#4099,.T.) ;
#3168 = FACE_OUTER_BOUND('',#4100,.T.) ;
#3169 = FACE_OUTER_BOUND('',#4101,.T.) ;
#3170 = FACE_OUTER_BOUND('',#4102,.T.) ;
#3171 = FACE_OUTER_BOUND('',#4103,.T.) ;
#3172 = FACE_OUTER_BOUND('',#4104,.T.) ;
#3173 = FACE_OUTER_BOUND('',#4105,.T.) ;
#3174 = FACE_OUTER_BOUND('',#4106,.T.) ;
#3175 = FACE_OUTER_BOUND('',#4107,.T.) ;
#3176 = FACE_OUTER_BOUND('',#4108,.T.) ;
#3177 = FACE_OUTER_BOUND('',#4109,.T.) ;
#3178 = FACE_OUTER_BOUND('',#4110,.T.) ;
#3179 = FACE_OUTER_BOUND('',#4111,.T.) ;
#3180 = FACE_OUTER_BOUND('',#4112,.T.) ;
#3181 = FACE_OUTER_BOUND('',#4113,.T.) ;
#3182 = FACE_OUTER_BOUND('',#4114,.T.) ;
#3183 = FACE_OUTER_BOUND('',#4115,.T.) ;
#3184 = FACE_OUTER_BOUND('',#4116,.T.) ;
#3185 = FACE_OUTER_BOUND('',#4117,.T.) ;
#3186 = FACE_OUTER_BOUND('',#4118,.T.) ;
#3187 = FACE_OUTER_BOUND('',#4119,.T.) ;
#3188 = FACE_OUTER_BOUND('',#4120,.T.) ;
#3189 = FACE_OUTER_BOUND('',#4121,.T.) ;
#3190 = FACE_OUTER_BOUND('',#4122,.T.) ;
#3191 = FACE_OUTER_BOUND('',#4123,.T.) ;
#3192 = FACE_OUTER_BOUND('',#4124,.T.) ;
#3193 = FACE_OUTER_BOUND('',#4125,.T.) ;
#3194 = FACE_OUTER_BOUND('',#4126,.T.) ;
#3195 = FACE_OUTER_BOUND('',#4127,.T.) ;
#3196 = FACE_OUTER_BOUND('',#4128,.T.) ;
#3197 = FACE_OUTER_BOUND('',#4129,.T.) ;
#3198 = FACE_OUTER_BOUND('',#4130,.T.) ;
#3199 = FACE_OUTER_BOUND('',#4131,.T.) ;
#3200 = FACE_OUTER_BOUND('',#4132,.T.) ;
#3201 = FACE_OUTER_BOUND('',#4133,.T.) ;
#3202 = FACE_OUTER_BOUND('',#4134,.T.) ;
#3203 = FACE_OUTER_BOUND('',#4135,.T.) ;
#3204 = FACE_OUTER_BOUND('',#4136,.T.) ;
#3205 = FACE_OUTER_BOUND('',#4137,.T.) ;
#3206 = FACE_OUTER_BOUND('',#4139,.T.) ;
#3207 = FACE_OUTER_BOUND('',#4140,.T.) ;
#3208 = FACE_OUTER_BOUND('',#4141,.T.) ;
#3209 = FACE_OUTER_BOUND('',#4142,.T.) ;
#3210 = FACE_OUTER_BOUND('',#4143,.T.) ;
#3211 = FACE_OUTER_BOUND('',#4144,.T.) ;
#3212 = FACE_OUTER_BOUND('',#4145,.T.) ;
#3213 = FACE_OUTER_BOUND('',#4146,.T.) ;
#3214 = FACE_OUTER_BOUND('',#4147,.T.) ;
#3215 = FACE_OUTER_BOUND('',#4149,.T.) ;
#3216 = FACE_OUTER_BOUND('',#4151,.T.) ;
#3217 = FACE_OUTER_BOUND('',#4152,.T.) ;
#3218 = FACE_OUTER_BOUND('',#4153,.T.) ;
#3219 = FACE_OUTER_BOUND('',#4154,.T.) ;
#3220 = FACE_OUTER_BOUND('',#4155,.T.) ;
#3221 = FACE_OUTER_BOUND('',#4156,.T.) ;
#3222 = FACE_OUTER_BOUND('',#4157,.T.) ;
#3223 = FACE_OUTER_BOUND('',#4158,.T.) ;
#3224 = FACE_OUTER_BOUND('',#4159,.T.) ;
#3225 = FACE_OUTER_BOUND('',#4160,.T.) ;
#3226 = FACE_OUTER_BOUND('',#4161,.T.) ;
#3227 = FACE_OUTER_BOUND('',#4162,.T.) ;
#3228 = FACE_OUTER_BOUND('',#4163,.T.) ;
#3229 = FACE_OUTER_BOUND('',#4164,.T.) ;
#3230 = FACE_OUTER_BOUND('',#4165,.T.) ;
#3231 = FACE_OUTER_BOUND('',#4166,.T.) ;
#3232 = FACE_OUTER_BOUND('',#4167,.T.) ;
#3233 = FACE_OUTER_BOUND('',#4168,.T.) ;
#3234 = FACE_OUTER_BOUND('',#4169,.T.) ;
#3235 = FACE_OUTER_BOUND('',#4170,.T.) ;
#3236 = FACE_OUTER_BOUND('',#4172,.T.) ;
#3237 = FACE_OUTER_BOUND('',#4173,.T.) ;
#3238 = FACE_OUTER_BOUND('',#4174,.T.) ;
#3239 = FACE_OUTER_BOUND('',#4177,.T.) ;
#3240 = FACE_OUTER_BOUND('',#4178,.T.) ;
#3241 = FACE_OUTER_BOUND('',#4179,.T.) ;
#3242 = FACE_OUTER_BOUND('',#4180,.T.) ;
#3243 = FACE_OUTER_BOUND('',#4181,.T.) ;
#3244 = FACE_OUTER_BOUND('',#4182,.T.) ;
#3245 = FACE_OUTER_BOUND('',#4183,.T.) ;
#3246 = FACE_OUTER_BOUND('',#4184,.T.) ;
#3247 = FACE_OUTER_BOUND('',#4185,.T.) ;
#3248 = FACE_OUTER_BOUND('',#4186,.T.) ;
#3249 = FACE_OUTER_BOUND('',#4187,.T.) ;
#3250 = FACE_OUTER_BOUND('',#4188,.T.) ;
#3251 = FACE_OUTER_BOUND('',#4189,.T.) ;
#3252 = FACE_OUTER_BOUND('',#4190,.T.) ;
#3253 = FACE_OUTER_BOUND('',#4191,.T.) ;
#3254 = FACE_OUTER_BOUND('',#4192,.T.) ;
#3255 = FACE_OUTER_BOUND('',#4193,.T.) ;
#3256 = FACE_OUTER_BOUND('',#4194,.T.) ;
#3257 = FACE_OUTER_BOUND('',#4195,.T.) ;
#3258 = FACE_OUTER_BOUND('',#4196,.T.) ;
#3259 = FACE_OUTER_BOUND('',#4197,.T.) ;
#3260 = FACE_OUTER_BOUND('',#4198,.T.) ;
#3261 = FACE_OUTER_BOUND('',#4199,.T.) ;
#3262 = FACE_OUTER_BOUND('',#4200,.T.) ;
#3263 = FACE_OUTER_BOUND('',#4201,.T.) ;
#3264 = FACE_OUTER_BOUND('',#4202,.T.) ;
#3265 = FACE_OUTER_BOUND('',#4203,.T.) ;
#3266 = FACE_OUTER_BOUND('',#4204,.T.) ;
#3267 = FACE_OUTER_BOUND('',#4205,.T.) ;
#3268 = FACE_OUTER_BOUND('',#4206,.T.) ;
#3269 = FACE_OUTER_BOUND('',#4207,.T.) ;
#3270 = FACE_OUTER_BOUND('',#4208,.T.) ;
#3271 = FACE_OUTER_BOUND('',#4209,.T.) ;
#3272 = FACE_OUTER_BOUND('',#4210,.T.) ;
#3273 = FACE_OUTER_BOUND('',#4211,.T.) ;
#3274 = FACE_OUTER_BOUND('',#4212,.T.) ;
#3275 = FACE_OUTER_BOUND('',#4213,.T.) ;
#3276 = FACE_OUTER_BOUND('',#4214,.T.) ;
#3277 = FACE_OUTER_BOUND('',#4215,.T.) ;
#3278 = FACE_OUTER_BOUND('',#4216,.T.) ;
#3279 = FACE_OUTER_BOUND('',#4217,.T.) ;
#3280 = FACE_OUTER_BOUND('',#4218,.T.) ;
#3281 = FACE_OUTER_BOUND('',#4219,.T.) ;
#3282 = FACE_OUTER_BOUND('',#4220,.T.) ;
#3283 = FACE_OUTER_BOUND('',#4221,.T.) ;
#3284 = FACE_OUTER_BOUND('',#4222,.T.) ;
#3285 = FACE_OUTER_BOUND('',#4223,.T.) ;
#3286 = FACE_OUTER_BOUND('',#4224,.T.) ;
#3287 = FACE_OUTER_BOUND('',#4225,.T.) ;
#3288 = FACE_OUTER_BOUND('',#4226,.T.) ;
#3289 = FACE_OUTER_BOUND('',#4227,.T.) ;
#3290 = FACE_OUTER_BOUND('',#4228,.T.) ;
#3291 = FACE_OUTER_BOUND('',#4229,.T.) ;
#3292 = FACE_OUTER_BOUND('',#4230,.T.) ;
#3293 = FACE_OUTER_BOUND('',#4231,.T.) ;
#3294 = FACE_OUTER_BOUND('',#4232,.T.) ;
#3295 = FACE_OUTER_BOUND('',#4233,.T.) ;
#3296 = FACE_OUTER_BOUND('',#4234,.T.) ;
#3297 = FACE_OUTER_BOUND('',#4235,.T.) ;
#3298 = FACE_OUTER_BOUND('',#4236,.T.) ;
#3299 = FACE_OUTER_BOUND('',#4237,.T.) ;
#3300 = FACE_OUTER_BOUND('',#4238,.T.) ;
#3301 = FACE_OUTER_BOUND('',#4239,.T.) ;
#3302 = FACE_OUTER_BOUND('',#4240,.T.) ;
#3303 = FACE_OUTER_BOUND('',#4241,.T.) ;
#3304 = FACE_OUTER_BOUND('',#4242,.T.) ;
#3305 = FACE_OUTER_BOUND('',#4243,.T.) ;
#3306 = FACE_OUTER_BOUND('',#4244,.T.) ;
#3307 = FACE_OUTER_BOUND('',#4245,.T.) ;
#3308 = FACE_OUTER_BOUND('',#4246,.T.) ;
#3309 = FACE_OUTER_BOUND('',#4247,.T.) ;
#3310 = FACE_OUTER_BOUND('',#4248,.T.) ;
#3311 = FACE_OUTER_BOUND('',#4249,.T.) ;
#3312 = FACE_OUTER_BOUND('',#4250,.T.) ;
#3313 = FACE_OUTER_BOUND('',#4251,.T.) ;
#3314 = FACE_OUTER_BOUND('',#4252,.T.) ;
#3315 = FACE_OUTER_BOUND('',#4253,.T.) ;
#3316 = FACE_OUTER_BOUND('',#4254,.T.) ;
#3317 = FACE_OUTER_BOUND('',#4255,.T.) ;
#3318 = FACE_OUTER_BOUND('',#4256,.T.) ;
#3319 = FACE_OUTER_BOUND('',#4257,.T.) ;
#3320 = FACE_OUTER_BOUND('',#4258,.T.) ;
#3321 = FACE_OUTER_BOUND('',#4259,.T.) ;
#3322 = FACE_OUTER_BOUND('',#4260,.T.) ;
#3323 = FACE_OUTER_BOUND('',#4261,.T.) ;
#3324 = FACE_OUTER_BOUND('',#4262,.T.) ;
#3325 = FACE_OUTER_BOUND('',#4263,.T.) ;
#3326 = FACE_OUTER_BOUND('',#4264,.T.) ;
#3327 = FACE_OUTER_BOUND('',#4265,.T.) ;
#3328 = FACE_OUTER_BOUND('',#4266,.T.) ;
#3329 = FACE_OUTER_BOUND('',#4267,.T.) ;
#3330 = FACE_OUTER_BOUND('',#4268,.T.) ;
#3331 = FACE_OUTER_BOUND('',#4269,.T.) ;
#3332 = FACE_OUTER_BOUND('',#4270,.T.) ;
#3333 = FACE_OUTER_BOUND('',#4271,.T.) ;
#3334 = FACE_OUTER_BOUND('',#4272,.T.) ;
#3335 = FACE_OUTER_BOUND('',#4273,.T.) ;
#3336 = FACE_OUTER_BOUND('',#4274,.T.) ;
#3337 = FACE_OUTER_BOUND('',#4275,.T.) ;
#3338 = FACE_OUTER_BOUND('',#4276,.T.) ;
#3339 = FACE_OUTER_BOUND('',#4277,.T.) ;
#3340 = FACE_OUTER_BOUND('',#4278,.T.) ;
#3341 = FACE_OUTER_BOUND('',#4279,.T.) ;
#3342 = FACE_OUTER_BOUND('',#4280,.T.) ;
#3343 = FACE_OUTER_BOUND('',#4281,.T.) ;
#3344 = FACE_OUTER_BOUND('',#4282,.T.) ;
#3345 = FACE_OUTER_BOUND('',#4283,.T.) ;
#3346 = FACE_OUTER_BOUND('',#4284,.T.) ;
#3347 = FACE_OUTER_BOUND('',#4285,.T.) ;
#3348 = FACE_OUTER_BOUND('',#4286,.T.) ;
#3349 = FACE_OUTER_BOUND('',#4287,.T.) ;
#3350 = FACE_OUTER_BOUND('',#4288,.T.) ;
#3351 = FACE_OUTER_BOUND('',#4289,.T.) ;
#3352 = FACE_OUTER_BOUND('',#4290,.T.) ;
#3353 = FACE_OUTER_BOUND('',#4292,.T.) ;
#3354 = FACE_OUTER_BOUND('',#4293,.T.) ;
#3355 = FACE_OUTER_BOUND('',#4294,.T.) ;
#3356 = FACE_OUTER_BOUND('',#4295,.T.) ;
#3357 = FACE_OUTER_BOUND('',#4296,.T.) ;
#3358 = FACE_OUTER_BOUND('',#4297,.T.) ;
#3359 = FACE_OUTER_BOUND('',#4299,.T.) ;
#3360 = FACE_OUTER_BOUND('',#4300,.T.) ;
#3361 = FACE_OUTER_BOUND('',#4302,.T.) ;
#3362 = FACE_OUTER_BOUND('',#4303,.T.) ;
#3363 = FACE_OUTER_BOUND('',#4304,.T.) ;
#3364 = FACE_OUTER_BOUND('',#4305,.T.) ;
#3365 = FACE_OUTER_BOUND('',#4306,.T.) ;
#3366 = FACE_OUTER_BOUND('',#4307,.T.) ;
#3367 = FACE_OUTER_BOUND('',#4308,.T.) ;
#3368 = FACE_OUTER_BOUND('',#4309,.T.) ;
#3369 = FACE_OUTER_BOUND('',#4310,.T.) ;
#3370 = FACE_OUTER_BOUND('',#4311,.T.) ;
#3371 = FACE_OUTER_BOUND('',#4312,.T.) ;
#3372 = FACE_OUTER_BOUND('',#4313,.T.) ;
#3373 = FACE_OUTER_BOUND('',#4314,.T.) ;
#3374 = FACE_OUTER_BOUND('',#4316,.T.) ;
#3375 = FACE_OUTER_BOUND('',#4317,.T.) ;
#3376 = FACE_OUTER_BOUND('',#4318,.T.) ;
#3377 = FACE_OUTER_BOUND('',#4319,.T.) ;
#3378 = FACE_OUTER_BOUND('',#4320,.T.) ;
#3379 = FACE_OUTER_BOUND('',#4321,.T.) ;
#3380 = FACE_OUTER_BOUND('',#4322,.T.) ;
#3381 = FACE_OUTER_BOUND('',#4323,.T.) ;
#3382 = FACE_OUTER_BOUND('',#4324,.T.) ;
#3383 = FACE_OUTER_BOUND('',#4325,.T.) ;
#3384 = FACE_OUTER_BOUND('',#4326,.T.) ;
#3385 = FACE_OUTER_BOUND('',#4327,.T.) ;
#3386 = FACE_OUTER_BOUND('',#4328,.T.) ;
#3387 = FACE_OUTER_BOUND('',#4330,.T.) ;
#3388 = FACE_OUTER_BOUND('',#4331,.T.) ;
#3389 = FACE_OUTER_BOUND('',#4332,.T.) ;
#3390 = FACE_OUTER_BOUND('',#4333,.T.) ;
#3391 = FACE_OUTER_BOUND('',#4334,.T.) ;
#3392 = FACE_OUTER_BOUND('',#4335,.T.) ;
#3393 = FACE_OUTER_BOUND('',#4336,.T.) ;
#3394 = FACE_OUTER_BOUND('',#4337,.T.) ;
#3395 = FACE_OUTER_BOUND('',#4338,.T.) ;
#3396 = FACE_OUTER_BOUND('',#4339,.T.) ;
#3397 = FACE_OUTER_BOUND('',#4340,.T.) ;
#3398 = FACE_OUTER_BOUND('',#4341,.T.) ;
#3399 = FACE_OUTER_BOUND('',#4342,.T.) ;
#3400 = FACE_OUTER_BOUND('',#4343,.T.) ;
#3401 = FACE_OUTER_BOUND('',#4344,.T.) ;
#3402 = FACE_OUTER_BOUND('',#4345,.T.) ;
#3403 = FACE_OUTER_BOUND('',#4346,.T.) ;
#3404 = FACE_OUTER_BOUND('',#4347,.T.) ;
#3405 = FACE_OUTER_BOUND('',#4349,.T.) ;
#3406 = FACE_OUTER_BOUND('',#4350,.T.) ;
#3407 = FACE_OUTER_BOUND('',#4351,.T.) ;
#3408 = FACE_OUTER_BOUND('',#4352,.T.) ;
#3409 = FACE_OUTER_BOUND('',#4353,.T.) ;
#3410 = FACE_OUTER_BOUND('',#4354,.T.) ;
#3411 = FACE_OUTER_BOUND('',#4355,.T.) ;
#3412 = FACE_OUTER_BOUND('',#4356,.T.) ;
#3413 = FACE_OUTER_BOUND('',#4357,.T.) ;
#3414 = FACE_OUTER_BOUND('',#4358,.T.) ;
#3415 = FACE_OUTER_BOUND('',#4359,.T.) ;
#3416 = FACE_OUTER_BOUND('',#4360,.T.) ;
#3417 = FACE_OUTER_BOUND('',#4361,.T.) ;
#3418 = FACE_OUTER_BOUND('',#4362,.T.) ;
#3419 = FACE_OUTER_BOUND('',#4363,.T.) ;
#3420 = FACE_OUTER_BOUND('',#4364,.T.) ;
#3421 = FACE_OUTER_BOUND('',#4365,.T.) ;
#3422 = FACE_OUTER_BOUND('',#4366,.T.) ;
#3423 = FACE_OUTER_BOUND('',#4367,.T.) ;
#3424 = FACE_OUTER_BOUND('',#4368,.T.) ;
#3425 = FACE_OUTER_BOUND('',#4369,.T.) ;
#3426 = FACE_OUTER_BOUND('',#4370,.T.) ;
#3427 = FACE_OUTER_BOUND('',#4371,.T.) ;
#3428 = FACE_OUTER_BOUND('',#4372,.T.) ;
#3429 = FACE_OUTER_BOUND('',#4373,.T.) ;
#3430 = FACE_OUTER_BOUND('',#4374,.T.) ;
#3431 = FACE_OUTER_BOUND('',#4375,.T.) ;
#3432 = FACE_OUTER_BOUND('',#4376,.T.) ;
#3433 = FACE_OUTER_BOUND('',#4377,.T.) ;
#3434 = FACE_OUTER_BOUND('',#4378,.T.) ;
#3435 = FACE_OUTER_BOUND('',#4379,.T.) ;
#3436 = FACE_OUTER_BOUND('',#4380,.T.) ;
#3437 = FACE_OUTER_BOUND('',#4381,.T.) ;
#3438 = FACE_OUTER_BOUND('',#4384,.T.) ;
#3439 = FACE_OUTER_BOUND('',#4385,.T.) ;
#3440 = FACE_OUTER_BOUND('',#4388,.T.) ;
#3441 = FACE_OUTER_BOUND('',#4389,.T.) ;
#3442 = FACE_OUTER_BOUND('',#4392,.T.) ;
#3443 = FACE_OUTER_BOUND('',#4393,.T.) ;
#3444 = FACE_OUTER_BOUND('',#4396,.T.) ;
#3445 = FACE_OUTER_BOUND('',#4397,.T.) ;
#3446 = FACE_OUTER_BOUND('',#4398,.T.) ;
#3447 = FACE_OUTER_BOUND('',#4399,.T.) ;
#3448 = FACE_OUTER_BOUND('',#4400,.T.) ;
#3449 = FACE_OUTER_BOUND('',#4401,.T.) ;
#3450 = FACE_OUTER_BOUND('',#4403,.T.) ;
#3451 = FACE_OUTER_BOUND('',#4405,.T.) ;
#3452 = FACE_OUTER_BOUND('',#4406,.T.) ;
#3453 = FACE_OUTER_BOUND('',#4407,.T.) ;
#3454 = FACE_OUTER_BOUND('',#4408,.T.) ;
#3455 = FACE_OUTER_BOUND('',#4409,.T.) ;
#3456 = FACE_OUTER_BOUND('',#4410,.T.) ;
#3457 = FACE_OUTER_BOUND('',#4411,.T.) ;
#3458 = FACE_OUTER_BOUND('',#4412,.T.) ;
#3459 = FACE_OUTER_BOUND('',#4413,.T.) ;
#3460 = FACE_OUTER_BOUND('',#4414,.T.) ;
#3461 = FACE_OUTER_BOUND('',#4415,.T.) ;
#3462 = FACE_OUTER_BOUND('',#4416,.T.) ;
#3463 = FACE_OUTER_BOUND('',#4418,.T.) ;
#3464 = FACE_OUTER_BOUND('',#4419,.T.) ;
#3465 = FACE_OUTER_BOUND('',#4420,.T.) ;
#3466 = FACE_OUTER_BOUND('',#4421,.T.) ;
#3467 = FACE_OUTER_BOUND('',#4422,.T.) ;
#3468 = FACE_OUTER_BOUND('',#4424,.T.) ;
#3469 = FACE_OUTER_BOUND('',#4426,.T.) ;
#3470 = FACE_OUTER_BOUND('',#4427,.T.) ;
#3471 = FACE_OUTER_BOUND('',#4428,.T.) ;
#3472 = FACE_OUTER_BOUND('',#4429,.T.) ;
#3473 = FACE_OUTER_BOUND('',#4430,.T.) ;
#3474 = FACE_OUTER_BOUND('',#4431,.T.) ;
#3475 = FACE_OUTER_BOUND('',#4432,.T.) ;
#3476 = FACE_OUTER_BOUND('',#4433,.T.) ;
#3477 = FACE_OUTER_BOUND('',#4434,.T.) ;
#3478 = FACE_OUTER_BOUND('',#4435,.T.) ;
#3479 = FACE_OUTER_BOUND('',#4436,.T.) ;
#3480 = FACE_OUTER_BOUND('',#4437,.T.) ;
#3481 = FACE_OUTER_BOUND('',#4438,.T.) ;
#3482 = FACE_OUTER_BOUND('',#4439,.T.) ;
#3483 = FACE_OUTER_BOUND('',#4440,.T.) ;
#3484 = FACE_OUTER_BOUND('',#4441,.T.) ;
#3485 = FACE_OUTER_BOUND('',#4442,.T.) ;
#3486 = FACE_OUTER_BOUND('',#4443,.T.) ;
#3487 = FACE_OUTER_BOUND('',#4444,.T.) ;
#3488 = FACE_OUTER_BOUND('',#4445,.T.) ;
#3489 = FACE_OUTER_BOUND('',#4446,.T.) ;
#3490 = FACE_OUTER_BOUND('',#4447,.T.) ;
#3491 = FACE_OUTER_BOUND('',#4448,.T.) ;
#3492 = FACE_OUTER_BOUND('',#4449,.T.) ;
#3493 = FACE_OUTER_BOUND('',#4450,.T.) ;
#3494 = FACE_OUTER_BOUND('',#4453,.T.) ;
#3495 = FACE_OUTER_BOUND('',#4455,.T.) ;
#3496 = FACE_OUTER_BOUND('',#4457,.T.) ;
#3497 = FACE_OUTER_BOUND('',#4458,.T.) ;
#3498 = FACE_OUTER_BOUND('',#4459,.T.) ;
#3499 = FACE_OUTER_BOUND('',#4461,.T.) ;
#3500 = FACE_OUTER_BOUND('',#4463,.T.) ;
#3501 = FACE_OUTER_BOUND('',#4465,.T.) ;
#3502 = FACE_OUTER_BOUND('',#4466,.T.) ;
#3503 = FACE_OUTER_BOUND('',#4468,.T.) ;
#3504 = FACE_OUTER_BOUND('',#4469,.T.) ;
#3505 = FACE_OUTER_BOUND('',#4470,.T.) ;
#3506 = FACE_OUTER_BOUND('',#4471,.T.) ;
#3507 = FACE_OUTER_BOUND('',#4473,.T.) ;
#3508 = FACE_OUTER_BOUND('',#4474,.T.) ;
#3509 = FACE_OUTER_BOUND('',#4475,.T.) ;
#3510 = FACE_OUTER_BOUND('',#4476,.T.) ;
#3511 = FACE_OUTER_BOUND('',#4477,.T.) ;
#3512 = FACE_OUTER_BOUND('',#4478,.T.) ;
#3513 = FACE_OUTER_BOUND('',#4479,.T.) ;
#3514 = FACE_OUTER_BOUND('',#4480,.T.) ;
#3515 = FACE_OUTER_BOUND('',#4481,.T.) ;
#3516 = FACE_OUTER_BOUND('',#4482,.T.) ;
#3517 = FACE_OUTER_BOUND('',#4483,.T.) ;
#3518 = FACE_OUTER_BOUND('',#4484,.T.) ;
#3519 = FACE_OUTER_BOUND('',#4485,.T.) ;
#3520 = FACE_OUTER_BOUND('',#4486,.T.) ;
#3521 = FACE_OUTER_BOUND('',#4487,.T.) ;
#3522 = FACE_OUTER_BOUND('',#4489,.T.) ;
#3523 = FACE_OUTER_BOUND('',#4490,.T.) ;
#3524 = FACE_OUTER_BOUND('',#4491,.T.) ;
#3525 = FACE_OUTER_BOUND('',#4492,.T.) ;
#3526 = FACE_OUTER_BOUND('',#4493,.T.) ;
#3527 = FACE_OUTER_BOUND('',#4494,.T.) ;
#3528 = FACE_OUTER_BOUND('',#4495,.T.) ;
#3529 = FACE_OUTER_BOUND('',#4497,.T.) ;
#3530 = FACE_OUTER_BOUND('',#4499,.T.) ;
#3531 = FACE_OUTER_BOUND('',#4500,.T.) ;
#3532 = FACE_OUTER_BOUND('',#4501,.T.) ;
#3533 = FACE_OUTER_BOUND('',#4503,.T.) ;
#3534 = FACE_OUTER_BOUND('',#4504,.T.) ;
#3535 = FACE_OUTER_BOUND('',#4505,.T.) ;
#3536 = FACE_OUTER_BOUND('',#4506,.T.) ;
#3537 = FACE_OUTER_BOUND('',#4507,.T.) ;
#3538 = FACE_OUTER_BOUND('',#4508,.T.) ;
#3539 = FACE_OUTER_BOUND('',#4509,.T.) ;
#3540 = FACE_OUTER_BOUND('',#4510,.T.) ;
#3541 = FACE_OUTER_BOUND('',#4511,.T.) ;
#3542 = FACE_OUTER_BOUND('',#4512,.T.) ;
#3543 = FACE_OUTER_BOUND('',#4513,.T.) ;
#3544 = FACE_OUTER_BOUND('',#4514,.T.) ;
#3545 = FACE_OUTER_BOUND('',#4515,.T.) ;
#3546 = FACE_OUTER_BOUND('',#4516,.T.) ;
#3547 = FACE_OUTER_BOUND('',#4517,.T.) ;
#3548 = FACE_OUTER_BOUND('',#4518,.T.) ;
#3549 = FACE_OUTER_BOUND('',#4519,.T.) ;
#3550 = FACE_OUTER_BOUND('',#4520,.T.) ;
#3551 = FACE_OUTER_BOUND('',#4521,.T.) ;
#3552 = FACE_OUTER_BOUND('',#4522,.T.) ;
#3553 = FACE_OUTER_BOUND('',#4523,.T.) ;
#3554 = FACE_OUTER_BOUND('',#4524,.T.) ;
#3555 = FACE_OUTER_BOUND('',#4525,.T.) ;
#3556 = FACE_OUTER_BOUND('',#4526,.T.) ;
#3557 = FACE_OUTER_BOUND('',#4527,.T.) ;
#3558 = FACE_OUTER_BOUND('',#4528,.T.) ;
#3559 = FACE_OUTER_BOUND('',#4529,.T.) ;
#3560 = FACE_OUTER_BOUND('',#4530,.T.) ;
#3561 = FACE_OUTER_BOUND('',#4531,.T.) ;
#3562 = FACE_OUTER_BOUND('',#4532,.T.) ;
#3563 = FACE_OUTER_BOUND('',#4533,.T.) ;
#3564 = FACE_OUTER_BOUND('',#4534,.T.) ;
#3565 = FACE_OUTER_BOUND('',#4535,.T.) ;
#3566 = FACE_OUTER_BOUND('',#4536,.T.) ;
#3567 = FACE_OUTER_BOUND('',#4537,.T.) ;
#3568 = FACE_OUTER_BOUND('',#4538,.T.) ;
#3569 = FACE_OUTER_BOUND('',#4539,.T.) ;
#3570 = FACE_OUTER_BOUND('',#4540,.T.) ;
#3571 = FACE_OUTER_BOUND('',#4541,.T.) ;
#3572 = FACE_OUTER_BOUND('',#4542,.T.) ;
#3573 = FACE_OUTER_BOUND('',#4543,.T.) ;
#3574 = FACE_OUTER_BOUND('',#4544,.T.) ;
#3575 = FACE_OUTER_BOUND('',#4545,.T.) ;
#3576 = FACE_OUTER_BOUND('',#4546,.T.) ;
#3577 = FACE_OUTER_BOUND('',#4547,.T.) ;
#3578 = FACE_OUTER_BOUND('',#4548,.T.) ;
#3579 = FACE_OUTER_BOUND('',#4549,.T.) ;
#3580 = FACE_OUTER_BOUND('',#4550,.T.) ;
#3581 = FACE_OUTER_BOUND('',#4551,.T.) ;
#3582 = FACE_OUTER_BOUND('',#4552,.T.) ;
#3583 = FACE_OUTER_BOUND('',#4553,.T.) ;
#3584 = FACE_OUTER_BOUND('',#4563,.T.) ;
#3585 = FACE_OUTER_BOUND('',#4565,.T.) ;
#3586 = FACE_OUTER_BOUND('',#4567,.T.) ;
#3587 = FACE_OUTER_BOUND('',#4568,.T.) ;
#3588 = FACE_OUTER_BOUND('',#4569,.T.) ;
#3589 = FACE_OUTER_BOUND('',#4571,.T.) ;
#3590 = FACE_OUTER_BOUND('',#4573,.T.) ;
#3591 = FACE_OUTER_BOUND('',#4574,.T.) ;
#3592 = FACE_OUTER_BOUND('',#4575,.T.) ;
#3593 = FACE_OUTER_BOUND('',#4576,.T.) ;
#3594 = FACE_OUTER_BOUND('',#4578,.T.) ;
#3595 = FACE_OUTER_BOUND('',#4579,.T.) ;
#3596 = FACE_OUTER_BOUND('',#4580,.T.) ;
#3597 = FACE_OUTER_BOUND('',#4581,.T.) ;
#3598 = FACE_OUTER_BOUND('',#4582,.T.) ;
#3599 = FACE_OUTER_BOUND('',#4583,.T.) ;
#3600 = FACE_OUTER_BOUND('',#4584,.T.) ;
#3601 = FACE_OUTER_BOUND('',#4585,.T.) ;
#3602 = FACE_OUTER_BOUND('',#4586,.T.) ;
#3603 = FACE_OUTER_BOUND('',#4587,.T.) ;
#3604 = FACE_OUTER_BOUND('',#4588,.T.) ;
#3605 = FACE_OUTER_BOUND('',#4589,.T.) ;
#3606 = FACE_OUTER_BOUND('',#4591,.T.) ;
#3607 = FACE_OUTER_BOUND('',#4592,.T.) ;
#3608 = FACE_OUTER_BOUND('',#4593,.T.) ;
#3609 = FACE_OUTER_BOUND('',#4594,.T.) ;
#3610 = FACE_OUTER_BOUND('',#4595,.T.) ;
#3611 = FACE_OUTER_BOUND('',#4597,.T.) ;
#3612 = FACE_OUTER_BOUND('',#4598,.T.) ;
#3613 = FACE_OUTER_BOUND('',#4599,.T.) ;
#3614 = FACE_OUTER_BOUND('',#4601,.T.) ;
#3615 = FACE_OUTER_BOUND('',#4602,.T.) ;
#3616 = FACE_OUTER_BOUND('',#4603,.T.) ;
#3617 = FACE_OUTER_BOUND('',#4604,.T.) ;
#3618 = FACE_OUTER_BOUND('',#4605,.T.) ;
#3619 = FACE_OUTER_BOUND('',#4606,.T.) ;
#3620 = FACE_OUTER_BOUND('',#4607,.T.) ;
#3621 = FACE_OUTER_BOUND('',#4609,.T.) ;
#3622 = FACE_OUTER_BOUND('',#4611,.T.) ;
#3623 = FACE_OUTER_BOUND('',#4612,.T.) ;
#3624 = FACE_OUTER_BOUND('',#4613,.T.) ;
#3625 = FACE_OUTER_BOUND('',#4614,.T.) ;
#3626 = FACE_OUTER_BOUND('',#4616,.T.) ;
#3627 = FACE_OUTER_BOUND('',#4618,.T.) ;
#3628 = FACE_OUTER_BOUND('',#4619,.T.) ;
#3629 = FACE_OUTER_BOUND('',#4620,.T.) ;
#3630 = FACE_OUTER_BOUND('',#4621,.T.) ;
#3631 = FACE_OUTER_BOUND('',#4622,.T.) ;
#3632 = FACE_OUTER_BOUND('',#4623,.T.) ;
#3633 = FACE_OUTER_BOUND('',#4624,.T.) ;
#3634 = FACE_OUTER_BOUND('',#4626,.T.) ;
#3635 = FACE_OUTER_BOUND('',#4627,.T.) ;
#3636 = FACE_OUTER_BOUND('',#4628,.T.) ;
#3637 = FACE_OUTER_BOUND('',#4630,.T.) ;
#3638 = FACE_OUTER_BOUND('',#4631,.T.) ;
#3639 = FACE_OUTER_BOUND('',#4632,.T.) ;
#3640 = FACE_OUTER_BOUND('',#4634,.T.) ;
#3641 = FACE_OUTER_BOUND('',#4636,.T.) ;
#3642 = FACE_OUTER_BOUND('',#4637,.T.) ;
#3643 = FACE_OUTER_BOUND('',#4638,.T.) ;
#3644 = FACE_OUTER_BOUND('',#4639,.T.) ;
#3645 = FACE_OUTER_BOUND('',#4640,.T.) ;
#3646 = FACE_OUTER_BOUND('',#4641,.T.) ;
#3647 = FACE_OUTER_BOUND('',#4642,.T.) ;
#3648 = FACE_OUTER_BOUND('',#4648,.T.) ;
#3649 = FACE_OUTER_BOUND('',#4654,.T.) ;
#3650 = FACE_OUTER_BOUND('',#4655,.T.) ;
#3651 = FACE_OUTER_BOUND('',#4656,.T.) ;
#3652 = FACE_OUTER_BOUND('',#4657,.T.) ;
#3653 = FACE_OUTER_BOUND('',#4658,.T.) ;
#3654 = FACE_OUTER_BOUND('',#4659,.T.) ;
#3655 = FACE_OUTER_BOUND('',#4660,.T.) ;
#3656 = FACE_OUTER_BOUND('',#4666,.T.) ;
#3657 = FACE_OUTER_BOUND('',#4672,.T.) ;
#3658 = FACE_OUTER_BOUND('',#4673,.T.) ;
#3659 = FACE_OUTER_BOUND('',#4674,.T.) ;
#3660 = FACE_OUTER_BOUND('',#4675,.T.) ;
#3661 = FACE_OUTER_BOUND('',#4676,.T.) ;
#3662 = FACE_OUTER_BOUND('',#4677,.T.) ;
#3663 = FACE_OUTER_BOUND('',#4678,.T.) ;
#3664 = FACE_OUTER_BOUND('',#4680,.T.) ;
#3665 = FACE_OUTER_BOUND('',#4682,.T.) ;
#3666 = FACE_OUTER_BOUND('',#4685,.T.) ;
#3667 = FACE_OUTER_BOUND('',#4686,.T.) ;
#3668 = FACE_OUTER_BOUND('',#4687,.T.) ;
#3669 = FACE_OUTER_BOUND('',#4689,.T.) ;
#3670 = FACE_OUTER_BOUND('',#4692,.T.) ;
#3671 = FACE_OUTER_BOUND('',#4693,.T.) ;
#3672 = FACE_OUTER_BOUND('',#4695,.T.) ;
#3673 = FACE_OUTER_BOUND('',#4696,.T.) ;
#3674 = FACE_OUTER_BOUND('',#4697,.T.) ;
#3675 = FACE_OUTER_BOUND('',#4698,.T.) ;
#3676 = FACE_OUTER_BOUND('',#4699,.T.) ;
#3677 = FACE_OUTER_BOUND('',#4701,.T.) ;
#3678 = FACE_OUTER_BOUND('',#4702,.T.) ;
#3679 = FACE_OUTER_BOUND('',#4703,.T.) ;
#3680 = FACE_OUTER_BOUND('',#4705,.T.) ;
#3681 = FACE_OUTER_BOUND('',#4707,.T.) ;
#3682 = FACE_OUTER_BOUND('',#4708,.T.) ;
#3683 = FACE_OUTER_BOUND('',#4709,.T.) ;
#3684 = FACE_OUTER_BOUND('',#4710,.T.) ;
#3685 = FACE_OUTER_BOUND('',#4712,.T.) ;
#3686 = FACE_OUTER_BOUND('',#4713,.T.) ;
#3687 = FACE_OUTER_BOUND('',#4714,.T.) ;
#3688 = FACE_OUTER_BOUND('',#4715,.T.) ;
#3689 = FACE_OUTER_BOUND('',#4716,.T.) ;
#3690 = FACE_OUTER_BOUND('',#4718,.T.) ;
#3691 = FACE_OUTER_BOUND('',#4719,.T.) ;
#3692 = FACE_OUTER_BOUND('',#4720,.T.) ;
#3693 = FACE_OUTER_BOUND('',#4721,.T.) ;
#3694 = FACE_OUTER_BOUND('',#4722,.T.) ;
#3695 = FACE_OUTER_BOUND('',#4723,.T.) ;
#3696 = FACE_OUTER_BOUND('',#4724,.T.) ;
#3697 = FACE_OUTER_BOUND('',#4725,.T.) ;
#3698 = FACE_OUTER_BOUND('',#4726,.T.) ;
#3699 = FACE_OUTER_BOUND('',#4727,.T.) ;
#3700 = FACE_OUTER_BOUND('',#4729,.T.) ;
#3701 = FACE_OUTER_BOUND('',#4730,.T.) ;
#3702 = FACE_OUTER_BOUND('',#4731,.T.) ;
#3703 = FACE_OUTER_BOUND('',#4732,.T.) ;
#3704 = FACE_OUTER_BOUND('',#4733,.T.) ;
#3705 = FACE_OUTER_BOUND('',#4734,.T.) ;
#3706 = FACE_OUTER_BOUND('',#4735,.T.) ;
#3707 = FACE_OUTER_BOUND('',#4736,.T.) ;
#3708 = FACE_OUTER_BOUND('',#4737,.T.) ;
#3709 = FACE_OUTER_BOUND('',#4738,.T.) ;
#3710 = FACE_OUTER_BOUND('',#4740,.T.) ;
#3711 = FACE_OUTER_BOUND('',#4741,.T.) ;
#3712 = FACE_OUTER_BOUND('',#4742,.T.) ;
#3713 = FACE_OUTER_BOUND('',#4743,.T.) ;
#3714 = FACE_OUTER_BOUND('',#4745,.T.) ;
#3715 = FACE_OUTER_BOUND('',#4746,.T.) ;
#3716 = FACE_OUTER_BOUND('',#4747,.T.) ;
#3717 = FACE_OUTER_BOUND('',#4748,.T.) ;
#3718 = FACE_OUTER_BOUND('',#4749,.T.) ;
#3719 = EDGE_LOOP('',(#8487,#8488,#8489)) ;
#3720 = EDGE_LOOP('',(#8490,#8491,#8492,#8493,#8494,#8495,#8496,#8497)) ;
#3721 = EDGE_LOOP('',(#8498,#8499,#8500,#8501,#8502,#8503,#8504,#8505,#8506,
#8507,#8508,#8509,#8510,#8511,#8512,#8513)) ;
#3722 = EDGE_LOOP('',(#8514,#8515,#8516,#8517,#8518)) ;
#3723 = EDGE_LOOP('',(#8519,#8520,#8521,#8522,#8523,#8524,#8525,#8526)) ;
#3724 = EDGE_LOOP('',(#8527,#8528,#8529)) ;
#3725 = EDGE_LOOP('',(#8530,#8531,#8532,#8533,#8534,#8535,#8536,#8537)) ;
#3726 = EDGE_LOOP('',(#8538)) ;
#3727 = EDGE_LOOP('',(#8539,#8540,#8541,#8542)) ;
#3728 = EDGE_LOOP('',(#8543,#8544,#8545,#8546)) ;
#3729 = EDGE_LOOP('',(#8547,#8548,#8549,#8550)) ;
#3730 = EDGE_LOOP('',(#8551,#8552,#8553,#8554)) ;
#3731 = EDGE_LOOP('',(#8555,#8556,#8557,#8558)) ;
#3732 = EDGE_LOOP('',(#8559,#8560,#8561,#8562)) ;
#3733 = EDGE_LOOP('',(#8563,#8564,#8565,#8566,#8567,#8568)) ;
#3734 = EDGE_LOOP('',(#8569,#8570,#8571,#8572)) ;
#3735 = EDGE_LOOP('',(#8573,#8574,#8575)) ;
#3736 = EDGE_LOOP('',(#8576,#8577,#8578,#8579,#8580)) ;
#3737 = EDGE_LOOP('',(#8581,#8582,#8583,#8584)) ;
#3738 = EDGE_LOOP('',(#8585)) ;
#3739 = EDGE_LOOP('',(#8586)) ;
#3740 = EDGE_LOOP('',(#8587,#8588,#8589)) ;
#3741 = EDGE_LOOP('',(#8590,#8591,#8592,#8593,#8594,#8595)) ;
#3742 = EDGE_LOOP('',(#8596,#8597,#8598,#8599,#8600,#8601,#8602,#8603,#8604,
#8605,#8606,#8607,#8608)) ;
#3743 = EDGE_LOOP('',(#8609,#8610)) ;
#3744 = EDGE_LOOP('',(#8611,#8612,#8613,#8614,#8615,#8616)) ;
#3745 = EDGE_LOOP('',(#8617,#8618,#8619,#8620,#8621)) ;
#3746 = EDGE_LOOP('',(#8622,#8623)) ;
#3747 = EDGE_LOOP('',(#8624)) ;
#3748 = EDGE_LOOP('',(#8625)) ;
#3749 = EDGE_LOOP('',(#8626,#8627,#8628,#8629)) ;
#3750 = EDGE_LOOP('',(#8630,#8631)) ;
#3751 = EDGE_LOOP('',(#8632,#8633,#8634,#8635,#8636,#8637,#8638,#8639)) ;
#3752 = EDGE_LOOP('',(#8640,#8641)) ;
#3753 = EDGE_LOOP('',(#8642,#8643,#8644,#8645,#8646,#8647,#8648,#8649)) ;
#3754 = EDGE_LOOP('',(#8650)) ;
#3755 = EDGE_LOOP('',(#8651)) ;
#3756 = EDGE_LOOP('',(#8652,#8653,#8654,#8655,#8656,#8657,#8658,#8659)) ;
#3757 = EDGE_LOOP('',(#8660)) ;
#3758 = EDGE_LOOP('',(#8661)) ;
#3759 = EDGE_LOOP('',(#8662)) ;
#3760 = EDGE_LOOP('',(#8663)) ;
#3761 = EDGE_LOOP('',(#8664)) ;
#3762 = EDGE_LOOP('',(#8665)) ;
#3763 = EDGE_LOOP('',(#8666)) ;
#3764 = EDGE_LOOP('',(#8667,#8668,#8669,#8670)) ;
#3765 = EDGE_LOOP('',(#8671,#8672,#8673,#8674)) ;
#3766 = EDGE_LOOP('',(#8675)) ;
#3767 = EDGE_LOOP('',(#8676)) ;
#3768 = EDGE_LOOP('',(#8677,#8678,#8679,#8680)) ;
#3769 = EDGE_LOOP('',(#8681)) ;
#3770 = EDGE_LOOP('',(#8682)) ;
#3771 = EDGE_LOOP('',(#8683,#8684,#8685,#8686)) ;
#3772 = EDGE_LOOP('',(#8687)) ;
#3773 = EDGE_LOOP('',(#8688)) ;
#3774 = EDGE_LOOP('',(#8689,#8690,#8691,#8692)) ;
#3775 = EDGE_LOOP('',(#8693)) ;
#3776 = EDGE_LOOP('',(#8694)) ;
#3777 = EDGE_LOOP('',(#8695)) ;
#3778 = EDGE_LOOP('',(#8696)) ;
#3779 = EDGE_LOOP('',(#8697)) ;
#3780 = EDGE_LOOP('',(#8698)) ;
#3781 = EDGE_LOOP('',(#8699)) ;
#3782 = EDGE_LOOP('',(#8700)) ;
#3783 = EDGE_LOOP('',(#8701)) ;
#3784 = EDGE_LOOP('',(#8702)) ;
#3785 = EDGE_LOOP('',(#8703,#8704,#8705,#8706)) ;
#3786 = EDGE_LOOP('',(#8707,#8708,#8709,#8710)) ;
#3787 = EDGE_LOOP('',(#8711,#8712,#8713,#8714)) ;
#3788 = EDGE_LOOP('',(#8715,#8716,#8717,#8718)) ;
#3789 = EDGE_LOOP('',(#8719,#8720,#8721,#8722)) ;
#3790 = EDGE_LOOP('',(#8723,#8724,#8725,#8726)) ;
#3791 = EDGE_LOOP('',(#8727,#8728,#8729,#8730)) ;
#3792 = EDGE_LOOP('',(#8731,#8732,#8733,#8734)) ;
#3793 = EDGE_LOOP('',(#8735,#8736,#8737,#8738)) ;
#3794 = EDGE_LOOP('',(#8739)) ;
#3795 = EDGE_LOOP('',(#8740)) ;
#3796 = EDGE_LOOP('',(#8741,#8742,#8743,#8744)) ;
#3797 = EDGE_LOOP('',(#8745,#8746,#8747,#8748)) ;
#3798 = EDGE_LOOP('',(#8749)) ;
#3799 = EDGE_LOOP('',(#8750)) ;
#3800 = EDGE_LOOP('',(#8751,#8752,#8753,#8754)) ;
#3801 = EDGE_LOOP('',(#8755)) ;
#3802 = EDGE_LOOP('',(#8756)) ;
#3803 = EDGE_LOOP('',(#8757,#8758,#8759,#8760)) ;
#3804 = EDGE_LOOP('',(#8761,#8762,#8763,#8764)) ;
#3805 = EDGE_LOOP('',(#8765)) ;
#3806 = EDGE_LOOP('',(#8766)) ;
#3807 = EDGE_LOOP('',(#8767)) ;
#3808 = EDGE_LOOP('',(#8768)) ;
#3809 = EDGE_LOOP('',(#8769)) ;
#3810 = EDGE_LOOP('',(#8770,#8771,#8772,#8773)) ;
#3811 = EDGE_LOOP('',(#8774)) ;
#3812 = EDGE_LOOP('',(#8775)) ;
#3813 = EDGE_LOOP('',(#8776)) ;
#3814 = EDGE_LOOP('',(#8777)) ;
#3815 = EDGE_LOOP('',(#8778)) ;
#3816 = EDGE_LOOP('',(#8779)) ;
#3817 = EDGE_LOOP('',(#8780)) ;
#3818 = EDGE_LOOP('',(#8781)) ;
#3819 = EDGE_LOOP('',(#8782)) ;
#3820 = EDGE_LOOP('',(#8783)) ;
#3821 = EDGE_LOOP('',(#8784)) ;
#3822 = EDGE_LOOP('',(#8785)) ;
#3823 = EDGE_LOOP('',(#8786)) ;
#3824 = EDGE_LOOP('',(#8787)) ;
#3825 = EDGE_LOOP('',(#8788)) ;
#3826 = EDGE_LOOP('',(#8789)) ;
#3827 = EDGE_LOOP('',(#8790)) ;
#3828 = EDGE_LOOP('',(#8791)) ;
#3829 = EDGE_LOOP('',(#8792)) ;
#3830 = EDGE_LOOP('',(#8793,#8794,#8795,#8796)) ;
#3831 = EDGE_LOOP('',(#8797)) ;
#3832 = EDGE_LOOP('',(#8798)) ;
#3833 = EDGE_LOOP('',(#8799,#8800,#8801,#8802)) ;
#3834 = EDGE_LOOP('',(#8803,#8804,#8805,#8806)) ;
#3835 = EDGE_LOOP('',(#8807,#8808,#8809,#8810)) ;
#3836 = EDGE_LOOP('',(#8811,#8812,#8813,#8814)) ;
#3837 = EDGE_LOOP('',(#8815,#8816,#8817,#8818)) ;
#3838 = EDGE_LOOP('',(#8819,#8820,#8821,#8822)) ;
#3839 = EDGE_LOOP('',(#8823,#8824,#8825,#8826)) ;
#3840 = EDGE_LOOP('',(#8827,#8828,#8829,#8830)) ;
#3841 = EDGE_LOOP('',(#8831)) ;
#3842 = EDGE_LOOP('',(#8832)) ;
#3843 = EDGE_LOOP('',(#8833)) ;
#3844 = EDGE_LOOP('',(#8834)) ;
#3845 = EDGE_LOOP('',(#8835)) ;
#3846 = EDGE_LOOP('',(#8836)) ;
#3847 = EDGE_LOOP('',(#8837)) ;
#3848 = EDGE_LOOP('',(#8838)) ;
#3849 = EDGE_LOOP('',(#8839)) ;
#3850 = EDGE_LOOP('',(#8840)) ;
#3851 = EDGE_LOOP('',(#8841)) ;
#3852 = EDGE_LOOP('',(#8842)) ;
#3853 = EDGE_LOOP('',(#8843)) ;
#3854 = EDGE_LOOP('',(#8844)) ;
#3855 = EDGE_LOOP('',(#8845)) ;
#3856 = EDGE_LOOP('',(#8846)) ;
#3857 = EDGE_LOOP('',(#8847,#8848,#8849,#8850)) ;
#3858 = EDGE_LOOP('',(#8851,#8852,#8853,#8854)) ;
#3859 = EDGE_LOOP('',(#8855,#8856,#8857,#8858)) ;
#3860 = EDGE_LOOP('',(#8859,#8860,#8861,#8862)) ;
#3861 = EDGE_LOOP('',(#8863,#8864,#8865,#8866,#8867,#8868,#8869,#8870)) ;
#3862 = EDGE_LOOP('',(#8871,#8872,#8873,#8874)) ;
#3863 = EDGE_LOOP('',(#8875)) ;
#3864 = EDGE_LOOP('',(#8876)) ;
#3865 = EDGE_LOOP('',(#8877)) ;
#3866 = EDGE_LOOP('',(#8878)) ;
#3867 = EDGE_LOOP('',(#8879,#8880,#8881,#8882)) ;
#3868 = EDGE_LOOP('',(#8883,#8884,#8885,#8886)) ;
#3869 = EDGE_LOOP('',(#8887,#8888,#8889,#8890)) ;
#3870 = EDGE_LOOP('',(#8891,#8892,#8893,#8894)) ;
#3871 = EDGE_LOOP('',(#8895)) ;
#3872 = EDGE_LOOP('',(#8896)) ;
#3873 = EDGE_LOOP('',(#8897)) ;
#3874 = EDGE_LOOP('',(#8898)) ;
#3875 = EDGE_LOOP('',(#8899)) ;
#3876 = EDGE_LOOP('',(#8900,#8901,#8902,#8903)) ;
#3877 = EDGE_LOOP('',(#8904,#8905,#8906,#8907)) ;
#3878 = EDGE_LOOP('',(#8908)) ;
#3879 = EDGE_LOOP('',(#8909,#8910,#8911,#8912,#8913)) ;
#3880 = EDGE_LOOP('',(#8914)) ;
#3881 = EDGE_LOOP('',(#8915)) ;
#3882 = EDGE_LOOP('',(#8916)) ;
#3883 = EDGE_LOOP('',(#8917)) ;
#3884 = EDGE_LOOP('',(#8918)) ;
#3885 = EDGE_LOOP('',(#8919,#8920,#8921,#8922)) ;
#3886 = EDGE_LOOP('',(#8923)) ;
#3887 = EDGE_LOOP('',(#8924,#8925,#8926,#8927)) ;
#3888 = EDGE_LOOP('',(#8928)) ;
#3889 = EDGE_LOOP('',(#8929,#8930,#8931,#8932)) ;
#3890 = EDGE_LOOP('',(#8933)) ;
#3891 = EDGE_LOOP('',(#8934,#8935,#8936,#8937)) ;
#3892 = EDGE_LOOP('',(#8938)) ;
#3893 = EDGE_LOOP('',(#8939,#8940,#8941,#8942)) ;
#3894 = EDGE_LOOP('',(#8943)) ;
#3895 = EDGE_LOOP('',(#8944,#8945,#8946,#8947)) ;
#3896 = EDGE_LOOP('',(#8948)) ;
#3897 = EDGE_LOOP('',(#8949,#8950,#8951,#8952)) ;
#3898 = EDGE_LOOP('',(#8953)) ;
#3899 = EDGE_LOOP('',(#8954,#8955,#8956,#8957)) ;
#3900 = EDGE_LOOP('',(#8958)) ;
#3901 = EDGE_LOOP('',(#8959,#8960,#8961,#8962)) ;
#3902 = EDGE_LOOP('',(#8963)) ;
#3903 = EDGE_LOOP('',(#8964,#8965,#8966,#8967)) ;
#3904 = EDGE_LOOP('',(#8968)) ;
#3905 = EDGE_LOOP('',(#8969,#8970,#8971,#8972)) ;
#3906 = EDGE_LOOP('',(#8973)) ;
#3907 = EDGE_LOOP('',(#8974,#8975,#8976,#8977)) ;
#3908 = EDGE_LOOP('',(#8978)) ;
#3909 = EDGE_LOOP('',(#8979,#8980,#8981,#8982)) ;
#3910 = EDGE_LOOP('',(#8983)) ;
#3911 = EDGE_LOOP('',(#8984,#8985,#8986,#8987)) ;
#3912 = EDGE_LOOP('',(#8988)) ;
#3913 = EDGE_LOOP('',(#8989,#8990,#8991,#8992)) ;
#3914 = EDGE_LOOP('',(#8993)) ;
#3915 = EDGE_LOOP('',(#8994,#8995,#8996,#8997)) ;
#3916 = EDGE_LOOP('',(#8998)) ;
#3917 = EDGE_LOOP('',(#8999,#9000,#9001,#9002)) ;
#3918 = EDGE_LOOP('',(#9003)) ;
#3919 = EDGE_LOOP('',(#9004,#9005,#9006,#9007)) ;
#3920 = EDGE_LOOP('',(#9008)) ;
#3921 = EDGE_LOOP('',(#9009,#9010,#9011,#9012)) ;
#3922 = EDGE_LOOP('',(#9013)) ;
#3923 = EDGE_LOOP('',(#9014,#9015,#9016,#9017)) ;
#3924 = EDGE_LOOP('',(#9018)) ;
#3925 = EDGE_LOOP('',(#9019,#9020,#9021,#9022)) ;
#3926 = EDGE_LOOP('',(#9023)) ;
#3927 = EDGE_LOOP('',(#9024,#9025,#9026,#9027)) ;
#3928 = EDGE_LOOP('',(#9028)) ;
#3929 = EDGE_LOOP('',(#9029,#9030,#9031,#9032)) ;
#3930 = EDGE_LOOP('',(#9033)) ;
#3931 = EDGE_LOOP('',(#9034,#9035,#9036,#9037)) ;
#3932 = EDGE_LOOP('',(#9038)) ;
#3933 = EDGE_LOOP('',(#9039,#9040,#9041,#9042)) ;
#3934 = EDGE_LOOP('',(#9043,#9044,#9045,#9046)) ;
#3935 = EDGE_LOOP('',(#9047,#9048,#9049,#9050)) ;
#3936 = EDGE_LOOP('',(#9051,#9052,#9053,#9054)) ;
#3937 = EDGE_LOOP('',(#9055,#9056,#9057,#9058)) ;
#3938 = EDGE_LOOP('',(#9059,#9060,#9061,#9062)) ;
#3939 = EDGE_LOOP('',(#9063,#9064,#9065,#9066)) ;
#3940 = EDGE_LOOP('',(#9067,#9068,#9069,#9070)) ;
#3941 = EDGE_LOOP('',(#9071,#9072,#9073,#9074)) ;
#3942 = EDGE_LOOP('',(#9075,#9076,#9077,#9078)) ;
#3943 = EDGE_LOOP('',(#9079,#9080,#9081,#9082)) ;
#3944 = EDGE_LOOP('',(#9083,#9084,#9085,#9086)) ;
#3945 = EDGE_LOOP('',(#9087,#9088,#9089,#9090)) ;
#3946 = EDGE_LOOP('',(#9091,#9092,#9093,#9094)) ;
#3947 = EDGE_LOOP('',(#9095,#9096,#9097,#9098)) ;
#3948 = EDGE_LOOP('',(#9099,#9100,#9101,#9102)) ;
#3949 = EDGE_LOOP('',(#9103,#9104,#9105,#9106)) ;
#3950 = EDGE_LOOP('',(#9107,#9108,#9109,#9110)) ;
#3951 = EDGE_LOOP('',(#9111,#9112,#9113,#9114)) ;
#3952 = EDGE_LOOP('',(#9115,#9116,#9117,#9118)) ;
#3953 = EDGE_LOOP('',(#9119,#9120,#9121,#9122)) ;
#3954 = EDGE_LOOP('',(#9123,#9124,#9125,#9126)) ;
#3955 = EDGE_LOOP('',(#9127,#9128,#9129,#9130)) ;
#3956 = EDGE_LOOP('',(#9131,#9132,#9133,#9134)) ;
#3957 = EDGE_LOOP('',(#9135,#9136,#9137,#9138)) ;
#3958 = EDGE_LOOP('',(#9139,#9140,#9141,#9142)) ;
#3959 = EDGE_LOOP('',(#9143,#9144,#9145,#9146)) ;
#3960 = EDGE_LOOP('',(#9147,#9148,#9149,#9150)) ;
#3961 = EDGE_LOOP('',(#9151,#9152,#9153,#9154)) ;
#3962 = EDGE_LOOP('',(#9155)) ;
#3963 = EDGE_LOOP('',(#9156)) ;
#3964 = EDGE_LOOP('',(#9157)) ;
#3965 = EDGE_LOOP('',(#9158)) ;
#3966 = EDGE_LOOP('',(#9159)) ;
#3967 = EDGE_LOOP('',(#9160)) ;
#3968 = EDGE_LOOP('',(#9161)) ;
#3969 = EDGE_LOOP('',(#9162)) ;
#3970 = EDGE_LOOP('',(#9163)) ;
#3971 = EDGE_LOOP('',(#9164)) ;
#3972 = EDGE_LOOP('',(#9165)) ;
#3973 = EDGE_LOOP('',(#9166)) ;
#3974 = EDGE_LOOP('',(#9167)) ;
#3975 = EDGE_LOOP('',(#9168)) ;
#3976 = EDGE_LOOP('',(#9169)) ;
#3977 = EDGE_LOOP('',(#9170)) ;
#3978 = EDGE_LOOP('',(#9171)) ;
#3979 = EDGE_LOOP('',(#9172)) ;
#3980 = EDGE_LOOP('',(#9173)) ;
#3981 = EDGE_LOOP('',(#9174)) ;
#3982 = EDGE_LOOP('',(#9175)) ;
#3983 = EDGE_LOOP('',(#9176)) ;
#3984 = EDGE_LOOP('',(#9177)) ;
#3985 = EDGE_LOOP('',(#9178)) ;
#3986 = EDGE_LOOP('',(#9179)) ;
#3987 = EDGE_LOOP('',(#9180)) ;
#3988 = EDGE_LOOP('',(#9181)) ;
#3989 = EDGE_LOOP('',(#9182)) ;
#3990 = EDGE_LOOP('',(#9183)) ;
#3991 = EDGE_LOOP('',(#9184)) ;
#3992 = EDGE_LOOP('',(#9185)) ;
#3993 = EDGE_LOOP('',(#9186)) ;
#3994 = EDGE_LOOP('',(#9187)) ;
#3995 = EDGE_LOOP('',(#9188)) ;
#3996 = EDGE_LOOP('',(#9189)) ;
#3997 = EDGE_LOOP('',(#9190)) ;
#3998 = EDGE_LOOP('',(#9191)) ;
#3999 = EDGE_LOOP('',(#9192)) ;
#4000 = EDGE_LOOP('',(#9193)) ;
#4001 = EDGE_LOOP('',(#9194)) ;
#4002 = EDGE_LOOP('',(#9195)) ;
#4003 = EDGE_LOOP('',(#9196)) ;
#4004 = EDGE_LOOP('',(#9197)) ;
#4005 = EDGE_LOOP('',(#9198)) ;
#4006 = EDGE_LOOP('',(#9199)) ;
#4007 = EDGE_LOOP('',(#9200)) ;
#4008 = EDGE_LOOP('',(#9201)) ;
#4009 = EDGE_LOOP('',(#9202)) ;
#4010 = EDGE_LOOP('',(#9203)) ;
#4011 = EDGE_LOOP('',(#9204)) ;
#4012 = EDGE_LOOP('',(#9205)) ;
#4013 = EDGE_LOOP('',(#9206)) ;
#4014 = EDGE_LOOP('',(#9207)) ;
#4015 = EDGE_LOOP('',(#9208)) ;
#4016 = EDGE_LOOP('',(#9209)) ;
#4017 = EDGE_LOOP('',(#9210)) ;
#4018 = EDGE_LOOP('',(#9211)) ;
#4019 = EDGE_LOOP('',(#9212)) ;
#4020 = EDGE_LOOP('',(#9213)) ;
#4021 = EDGE_LOOP('',(#9214)) ;
#4022 = EDGE_LOOP('',(#9215)) ;
#4023 = EDGE_LOOP('',(#9216)) ;
#4024 = EDGE_LOOP('',(#9217)) ;
#4025 = EDGE_LOOP('',(#9218)) ;
#4026 = EDGE_LOOP('',(#9219)) ;
#4027 = EDGE_LOOP('',(#9220)) ;
#4028 = EDGE_LOOP('',(#9221)) ;
#4029 = EDGE_LOOP('',(#9222)) ;
#4030 = EDGE_LOOP('',(#9223)) ;
#4031 = EDGE_LOOP('',(#9224)) ;
#4032 = EDGE_LOOP('',(#9225)) ;
#4033 = EDGE_LOOP('',(#9226)) ;
#4034 = EDGE_LOOP('',(#9227)) ;
#4035 = EDGE_LOOP('',(#9228)) ;
#4036 = EDGE_LOOP('',(#9229)) ;
#4037 = EDGE_LOOP('',(#9230)) ;
#4038 = EDGE_LOOP('',(#9231)) ;
#4039 = EDGE_LOOP('',(#9232)) ;
#4040 = EDGE_LOOP('',(#9233)) ;
#4041 = EDGE_LOOP('',(#9234)) ;
#4042 = EDGE_LOOP('',(#9235)) ;
#4043 = EDGE_LOOP('',(#9236)) ;
#4044 = EDGE_LOOP('',(#9237)) ;
#4045 = EDGE_LOOP('',(#9238)) ;
#4046 = EDGE_LOOP('',(#9239)) ;
#4047 = EDGE_LOOP('',(#9240)) ;
#4048 = EDGE_LOOP('',(#9241,#9242,#9243,#9244)) ;
#4049 = EDGE_LOOP('',(#9245,#9246,#9247,#9248)) ;
#4050 = EDGE_LOOP('',(#9249)) ;
#4051 = EDGE_LOOP('',(#9250)) ;
#4052 = EDGE_LOOP('',(#9251,#9252,#9253,#9254)) ;
#4053 = EDGE_LOOP('',(#9255)) ;
#4054 = EDGE_LOOP('',(#9256)) ;
#4055 = EDGE_LOOP('',(#9257,#9258,#9259,#9260)) ;
#4056 = EDGE_LOOP('',(#9261)) ;
#4057 = EDGE_LOOP('',(#9262)) ;
#4058 = EDGE_LOOP('',(#9263)) ;
#4059 = EDGE_LOOP('',(#9264)) ;
#4060 = EDGE_LOOP('',(#9265,#9266,#9267,#9268)) ;
#4061 = EDGE_LOOP('',(#9269,#9270,#9271,#9272)) ;
#4062 = EDGE_LOOP('',(#9273)) ;
#4063 = EDGE_LOOP('',(#9274)) ;
#4064 = EDGE_LOOP('',(#9275,#9276,#9277,#9278)) ;
#4065 = EDGE_LOOP('',(#9279)) ;
#4066 = EDGE_LOOP('',(#9280)) ;
#4067 = EDGE_LOOP('',(#9281,#9282,#9283,#9284)) ;
#4068 = EDGE_LOOP('',(#9285,#9286,#9287,#9288)) ;
#4069 = EDGE_LOOP('',(#9289,#9290,#9291,#9292)) ;
#4070 = EDGE_LOOP('',(#9293)) ;
#4071 = EDGE_LOOP('',(#9294)) ;
#4072 = EDGE_LOOP('',(#9295)) ;
#4073 = EDGE_LOOP('',(#9296)) ;
#4074 = EDGE_LOOP('',(#9297,#9298,#9299,#9300)) ;
#4075 = EDGE_LOOP('',(#9301,#9302,#9303,#9304)) ;
#4076 = EDGE_LOOP('',(#9305,#9306,#9307,#9308)) ;
#4077 = EDGE_LOOP('',(#9309,#9310,#9311,#9312)) ;
#4078 = EDGE_LOOP('',(#9313,#9314,#9315,#9316)) ;
#4079 = EDGE_LOOP('',(#9317,#9318,#9319,#9320)) ;
#4080 = EDGE_LOOP('',(#9321,#9322,#9323,#9324)) ;
#4081 = EDGE_LOOP('',(#9325,#9326,#9327,#9328)) ;
#4082 = EDGE_LOOP('',(#9329,#9330,#9331,#9332)) ;
#4083 = EDGE_LOOP('',(#9333)) ;
#4084 = EDGE_LOOP('',(#9334,#9335,#9336,#9337)) ;
#4085 = EDGE_LOOP('',(#9338,#9339,#9340,#9341)) ;
#4086 = EDGE_LOOP('',(#9342,#9343,#9344,#9345)) ;
#4087 = EDGE_LOOP('',(#9346,#9347,#9348,#9349)) ;
#4088 = EDGE_LOOP('',(#9350,#9351,#9352,#9353)) ;
#4089 = EDGE_LOOP('',(#9354,#9355,#9356,#9357)) ;
#4090 = EDGE_LOOP('',(#9358,#9359,#9360,#9361)) ;
#4091 = EDGE_LOOP('',(#9362,#9363,#9364,#9365,#9366,#9367,#9368,#9369,#9370,
#9371,#9372,#9373,#9374,#9375,#9376,#9377,#9378,#9379,#9380,#9381,#9382,
#9383,#9384,#9385,#9386,#9387,#9388,#9389,#9390,#9391,#9392,#9393,#9394,
#9395,#9396,#9397,#9398,#9399,#9400,#9401,#9402,#9403,#9404,#9405,#9406,
#9407,#9408,#9409)) ;
#4092 = EDGE_LOOP('',(#9410,#9411,#9412,#9413)) ;
#4093 = EDGE_LOOP('',(#9414,#9415,#9416,#9417)) ;
#4094 = EDGE_LOOP('',(#9418,#9419,#9420,#9421)) ;
#4095 = EDGE_LOOP('',(#9422,#9423,#9424,#9425)) ;
#4096 = EDGE_LOOP('',(#9426,#9427,#9428,#9429)) ;
#4097 = EDGE_LOOP('',(#9430,#9431,#9432,#9433)) ;
#4098 = EDGE_LOOP('',(#9434,#9435,#9436,#9437)) ;
#4099 = EDGE_LOOP('',(#9438,#9439,#9440,#9441)) ;
#4100 = EDGE_LOOP('',(#9442,#9443,#9444,#9445)) ;
#4101 = EDGE_LOOP('',(#9446,#9447,#9448,#9449)) ;
#4102 = EDGE_LOOP('',(#9450,#9451,#9452,#9453)) ;
#4103 = EDGE_LOOP('',(#9454,#9455,#9456,#9457)) ;
#4104 = EDGE_LOOP('',(#9458,#9459,#9460,#9461)) ;
#4105 = EDGE_LOOP('',(#9462,#9463,#9464,#9465)) ;
#4106 = EDGE_LOOP('',(#9466,#9467,#9468,#9469)) ;
#4107 = EDGE_LOOP('',(#9470,#9471,#9472,#9473)) ;
#4108 = EDGE_LOOP('',(#9474,#9475,#9476,#9477)) ;
#4109 = EDGE_LOOP('',(#9478,#9479,#9480,#9481)) ;
#4110 = EDGE_LOOP('',(#9482,#9483,#9484,#9485)) ;
#4111 = EDGE_LOOP('',(#9486,#9487,#9488,#9489)) ;
#4112 = EDGE_LOOP('',(#9490,#9491,#9492,#9493)) ;
#4113 = EDGE_LOOP('',(#9494,#9495,#9496,#9497)) ;
#4114 = EDGE_LOOP('',(#9498,#9499,#9500,#9501)) ;
#4115 = EDGE_LOOP('',(#9502,#9503,#9504,#9505)) ;
#4116 = EDGE_LOOP('',(#9506,#9507,#9508,#9509)) ;
#4117 = EDGE_LOOP('',(#9510,#9511,#9512,#9513)) ;
#4118 = EDGE_LOOP('',(#9514,#9515,#9516,#9517)) ;
#4119 = EDGE_LOOP('',(#9518,#9519,#9520,#9521)) ;
#4120 = EDGE_LOOP('',(#9522,#9523,#9524,#9525)) ;
#4121 = EDGE_LOOP('',(#9526,#9527,#9528,#9529)) ;
#4122 = EDGE_LOOP('',(#9530,#9531,#9532,#9533)) ;
#4123 = EDGE_LOOP('',(#9534,#9535,#9536,#9537)) ;
#4124 = EDGE_LOOP('',(#9538,#9539,#9540,#9541)) ;
#4125 = EDGE_LOOP('',(#9542,#9543,#9544,#9545)) ;
#4126 = EDGE_LOOP('',(#9546,#9547,#9548,#9549)) ;
#4127 = EDGE_LOOP('',(#9550,#9551,#9552,#9553)) ;
#4128 = EDGE_LOOP('',(#9554,#9555,#9556,#9557)) ;
#4129 = EDGE_LOOP('',(#9558,#9559,#9560,#9561)) ;
#4130 = EDGE_LOOP('',(#9562,#9563,#9564,#9565)) ;
#4131 = EDGE_LOOP('',(#9566,#9567,#9568,#9569)) ;
#4132 = EDGE_LOOP('',(#9570,#9571,#9572,#9573)) ;
#4133 = EDGE_LOOP('',(#9574,#9575,#9576,#9577)) ;
#4134 = EDGE_LOOP('',(#9578,#9579,#9580,#9581)) ;
#4135 = EDGE_LOOP('',(#9582,#9583,#9584,#9585)) ;
#4136 = EDGE_LOOP('',(#9586,#9587,#9588,#9589)) ;
#4137 = EDGE_LOOP('',(#9590,#9591,#9592,#9593,#9594,#9595,#9596,#9597,#9598,
#9599,#9600,#9601,#9602,#9603,#9604,#9605,#9606,#9607,#9608,#9609,#9610,
#9611,#9612,#9613,#9614,#9615,#9616,#9617,#9618,#9619,#9620,#9621,#9622,
#9623,#9624,#9625,#9626,#9627,#9628,#9629,#9630,#9631,#9632,#9633,#9634,
#9635,#9636,#9637)) ;
#4138 = EDGE_LOOP('',(#9638)) ;
#4139 = EDGE_LOOP('',(#9639,#9640,#9641,#9642)) ;
#4140 = EDGE_LOOP('',(#9643,#9644,#9645,#9646)) ;
#4141 = EDGE_LOOP('',(#9647,#9648,#9649,#9650)) ;
#4142 = EDGE_LOOP('',(#9651,#9652,#9653,#9654)) ;
#4143 = EDGE_LOOP('',(#9655,#9656,#9657,#9658)) ;
#4144 = EDGE_LOOP('',(#9659,#9660,#9661,#9662)) ;
#4145 = EDGE_LOOP('',(#9663,#9664,#9665,#9666)) ;
#4146 = EDGE_LOOP('',(#9667,#9668,#9669,#9670)) ;
#4147 = EDGE_LOOP('',(#9671)) ;
#4148 = EDGE_LOOP('',(#9672)) ;
#4149 = EDGE_LOOP('',(#9673)) ;
#4150 = EDGE_LOOP('',(#9674)) ;
#4151 = EDGE_LOOP('',(#9675,#9676,#9677,#9678)) ;
#4152 = EDGE_LOOP('',(#9679,#9680,#9681,#9682)) ;
#4153 = EDGE_LOOP('',(#9683,#9684,#9685,#9686)) ;
#4154 = EDGE_LOOP('',(#9687,#9688,#9689,#9690)) ;
#4155 = EDGE_LOOP('',(#9691,#9692,#9693,#9694,#9695,#9696,#9697,#9698)) ;
#4156 = EDGE_LOOP('',(#9699,#9700,#9701,#9702,#9703,#9704,#9705,#9706)) ;
#4157 = EDGE_LOOP('',(#9707,#9708,#9709,#9710)) ;
#4158 = EDGE_LOOP('',(#9711,#9712,#9713,#9714)) ;
#4159 = EDGE_LOOP('',(#9715,#9716,#9717,#9718)) ;
#4160 = EDGE_LOOP('',(#9719,#9720,#9721,#9722)) ;
#4161 = EDGE_LOOP('',(#9723,#9724,#9725,#9726)) ;
#4162 = EDGE_LOOP('',(#9727)) ;
#4163 = EDGE_LOOP('',(#9728,#9729,#9730,#9731)) ;
#4164 = EDGE_LOOP('',(#9732,#9733,#9734,#9735)) ;
#4165 = EDGE_LOOP('',(#9736,#9737,#9738,#9739)) ;
#4166 = EDGE_LOOP('',(#9740,#9741,#9742,#9743)) ;
#4167 = EDGE_LOOP('',(#9744,#9745,#9746,#9747)) ;
#4168 = EDGE_LOOP('',(#9748,#9749,#9750,#9751)) ;
#4169 = EDGE_LOOP('',(#9752,#9753,#9754,#9755)) ;
#4170 = EDGE_LOOP('',(#9756,#9757,#9758,#9759,#9760,#9761,#9762,#9763,#9764,
#9765)) ;
#4171 = EDGE_LOOP('',(#9766)) ;
#4172 = EDGE_LOOP('',(#9767,#9768,#9769,#9770)) ;
#4173 = EDGE_LOOP('',(#9771,#9772,#9773,#9774)) ;
#4174 = EDGE_LOOP('',(#9775,#9776,#9777,#9778,#9779,#9780,#9781,#9782,#9783,
#9784)) ;
#4175 = EDGE_LOOP('',(#9785)) ;
#4176 = EDGE_LOOP('',(#9786)) ;
#4177 = EDGE_LOOP('',(#9787,#9788,#9789,#9790)) ;
#4178 = EDGE_LOOP('',(#9791,#9792,#9793,#9794)) ;
#4179 = EDGE_LOOP('',(#9795,#9796,#9797,#9798)) ;
#4180 = EDGE_LOOP('',(#9799)) ;
#4181 = EDGE_LOOP('',(#9800)) ;
#4182 = EDGE_LOOP('',(#9801,#9802)) ;
#4183 = EDGE_LOOP('',(#9803,#9804,#9805,#9806,#9807,#9808)) ;
#4184 = EDGE_LOOP('',(#9809,#9810,#9811,#9812)) ;
#4185 = EDGE_LOOP('',(#9813,#9814,#9815,#9816)) ;
#4186 = EDGE_LOOP('',(#9817,#9818,#9819,#9820)) ;
#4187 = EDGE_LOOP('',(#9821,#9822,#9823,#9824,#9825,#9826)) ;
#4188 = EDGE_LOOP('',(#9827,#9828)) ;
#4189 = EDGE_LOOP('',(#9829,#9830)) ;
#4190 = EDGE_LOOP('',(#9831,#9832)) ;
#4191 = EDGE_LOOP('',(#9833,#9834,#9835,#9836,#9837,#9838)) ;
#4192 = EDGE_LOOP('',(#9839,#9840,#9841,#9842)) ;
#4193 = EDGE_LOOP('',(#9843,#9844,#9845,#9846)) ;
#4194 = EDGE_LOOP('',(#9847,#9848,#9849,#9850)) ;
#4195 = EDGE_LOOP('',(#9851,#9852,#9853,#9854,#9855,#9856)) ;
#4196 = EDGE_LOOP('',(#9857,#9858)) ;
#4197 = EDGE_LOOP('',(#9859,#9860)) ;
#4198 = EDGE_LOOP('',(#9861,#9862)) ;
#4199 = EDGE_LOOP('',(#9863,#9864,#9865,#9866,#9867,#9868)) ;
#4200 = EDGE_LOOP('',(#9869,#9870,#9871,#9872)) ;
#4201 = EDGE_LOOP('',(#9873,#9874,#9875,#9876)) ;
#4202 = EDGE_LOOP('',(#9877,#9878,#9879,#9880)) ;
#4203 = EDGE_LOOP('',(#9881,#9882,#9883,#9884,#9885,#9886)) ;
#4204 = EDGE_LOOP('',(#9887,#9888)) ;
#4205 = EDGE_LOOP('',(#9889,#9890)) ;
#4206 = EDGE_LOOP('',(#9891,#9892)) ;
#4207 = EDGE_LOOP('',(#9893,#9894,#9895,#9896,#9897,#9898)) ;
#4208 = EDGE_LOOP('',(#9899,#9900,#9901,#9902)) ;
#4209 = EDGE_LOOP('',(#9903,#9904,#9905,#9906)) ;
#4210 = EDGE_LOOP('',(#9907,#9908,#9909,#9910)) ;
#4211 = EDGE_LOOP('',(#9911,#9912,#9913,#9914,#9915,#9916)) ;
#4212 = EDGE_LOOP('',(#9917,#9918)) ;
#4213 = EDGE_LOOP('',(#9919,#9920,#9921,#9922,#9923,#9924,#9925)) ;
#4214 = EDGE_LOOP('',(#9926)) ;
#4215 = EDGE_LOOP('',(#9927,#9928,#9929,#9930,#9931,#9932,#9933,#9934,#9935)) ;
#4216 = EDGE_LOOP('',(#9936,#9937,#9938,#9939,#9940,#9941,#9942,#9943,#9944,
#9945)) ;
#4217 = EDGE_LOOP('',(#9946,#9947,#9948,#9949,#9950,#9951,#9952,#9953)) ;
#4218 = EDGE_LOOP('',(#9954,#9955,#9956,#9957,#9958,#9959,#9960,#9961)) ;
#4219 = EDGE_LOOP('',(#9962,#9963,#9964,#9965,#9966,#9967,#9968,#9969,#9970,
#9971)) ;
#4220 = EDGE_LOOP('',(#9972,#9973,#9974,#9975,#9976,#9977,#9978,#9979,#9980)) ;
#4221 = EDGE_LOOP('',(#9981,#9982,#9983,#9984,#9985,#9986,#9987,#9988,#9989)) ;
#4222 = EDGE_LOOP('',(#9990,#9991,#9992,#9993,#9994,#9995,#9996,#9997,#9998)) ;
#4223 = EDGE_LOOP('',(#9999,#10000,#10001,#10002,#10003,#10004,#10005,#10006,
#10007)) ;
#4224 = EDGE_LOOP('',(#10008,#10009,#10010,#10011,#10012,#10013,#10014,#10015,
#10016,#10017)) ;
#4225 = EDGE_LOOP('',(#10018,#10019,#10020,#10021,#10022,#10023,#10024,#10025)) ;
#4226 = EDGE_LOOP('',(#10026,#10027,#10028,#10029,#10030,#10031,#10032,#10033)) ;
#4227 = EDGE_LOOP('',(#10034,#10035,#10036,#10037,#10038,#10039,#10040,#10041,
#10042,#10043)) ;
#4228 = EDGE_LOOP('',(#10044,#10045,#10046,#10047,#10048,#10049,#10050,#10051,
#10052)) ;
#4229 = EDGE_LOOP('',(#10053,#10054,#10055,#10056,#10057,#10058,#10059,#10060,
#10061)) ;
#4230 = EDGE_LOOP('',(#10062,#10063,#10064,#10065,#10066,#10067,#10068,#10069,
#10070)) ;
#4231 = EDGE_LOOP('',(#10071,#10072,#10073,#10074,#10075,#10076,#10077,#10078,
#10079)) ;
#4232 = EDGE_LOOP('',(#10080,#10081,#10082,#10083,#10084,#10085,#10086,#10087,
#10088,#10089)) ;
#4233 = EDGE_LOOP('',(#10090,#10091,#10092,#10093,#10094,#10095,#10096,#10097)) ;
#4234 = EDGE_LOOP('',(#10098,#10099,#10100,#10101,#10102,#10103,#10104,#10105)) ;
#4235 = EDGE_LOOP('',(#10106,#10107,#10108,#10109,#10110,#10111,#10112,#10113,
#10114,#10115)) ;
#4236 = EDGE_LOOP('',(#10116,#10117,#10118,#10119,#10120,#10121,#10122,#10123,
#10124)) ;
#4237 = EDGE_LOOP('',(#10125,#10126,#10127,#10128,#10129,#10130,#10131,#10132,
#10133)) ;
#4238 = EDGE_LOOP('',(#10134,#10135,#10136,#10137,#10138,#10139,#10140,#10141,
#10142)) ;
#4239 = EDGE_LOOP('',(#10143,#10144,#10145,#10146,#10147,#10148,#10149,#10150,
#10151)) ;
#4240 = EDGE_LOOP('',(#10152,#10153,#10154,#10155,#10156,#10157,#10158,#10159,
#10160,#10161)) ;
#4241 = EDGE_LOOP('',(#10162,#10163,#10164,#10165,#10166,#10167,#10168,#10169)) ;
#4242 = EDGE_LOOP('',(#10170,#10171,#10172,#10173,#10174,#10175,#10176,#10177)) ;
#4243 = EDGE_LOOP('',(#10178,#10179,#10180,#10181,#10182,#10183,#10184,#10185,
#10186,#10187)) ;
#4244 = EDGE_LOOP('',(#10188,#10189,#10190,#10191,#10192,#10193,#10194,#10195,
#10196)) ;
#4245 = EDGE_LOOP('',(#10197,#10198,#10199,#10200,#10201,#10202,#10203)) ;
#4246 = EDGE_LOOP('',(#10204)) ;
#4247 = EDGE_LOOP('',(#10205,#10206,#10207)) ;
#4248 = EDGE_LOOP('',(#10208,#10209,#10210)) ;
#4249 = EDGE_LOOP('',(#10211,#10212,#10213)) ;
#4250 = EDGE_LOOP('',(#10214,#10215,#10216)) ;
#4251 = EDGE_LOOP('',(#10217,#10218)) ;
#4252 = EDGE_LOOP('',(#10219,#10220)) ;
#4253 = EDGE_LOOP('',(#10221,#10222)) ;
#4254 = EDGE_LOOP('',(#10223,#10224,#10225)) ;
#4255 = EDGE_LOOP('',(#10226,#10227,#10228,#10229,#10230)) ;
#4256 = EDGE_LOOP('',(#10231,#10232)) ;
#4257 = EDGE_LOOP('',(#10233,#10234)) ;
#4258 = EDGE_LOOP('',(#10235,#10236,#10237,#10238)) ;
#4259 = EDGE_LOOP('',(#10239,#10240,#10241)) ;
#4260 = EDGE_LOOP('',(#10242,#10243,#10244)) ;
#4261 = EDGE_LOOP('',(#10245,#10246,#10247)) ;
#4262 = EDGE_LOOP('',(#10248,#10249,#10250)) ;
#4263 = EDGE_LOOP('',(#10251,#10252,#10253)) ;
#4264 = EDGE_LOOP('',(#10254,#10255,#10256,#10257)) ;
#4265 = EDGE_LOOP('',(#10258,#10259,#10260)) ;
#4266 = EDGE_LOOP('',(#10261,#10262,#10263,#10264)) ;
#4267 = EDGE_LOOP('',(#10265,#10266,#10267)) ;
#4268 = EDGE_LOOP('',(#10268,#10269,#10270)) ;
#4269 = EDGE_LOOP('',(#10271,#10272,#10273)) ;
#4270 = EDGE_LOOP('',(#10274,#10275,#10276)) ;
#4271 = EDGE_LOOP('',(#10277,#10278,#10279)) ;
#4272 = EDGE_LOOP('',(#10280,#10281,#10282,#10283)) ;
#4273 = EDGE_LOOP('',(#10284,#10285,#10286)) ;
#4274 = EDGE_LOOP('',(#10287,#10288,#10289,#10290)) ;
#4275 = EDGE_LOOP('',(#10291,#10292,#10293)) ;
#4276 = EDGE_LOOP('',(#10294,#10295,#10296)) ;
#4277 = EDGE_LOOP('',(#10297,#10298,#10299)) ;
#4278 = EDGE_LOOP('',(#10300,#10301,#10302)) ;
#4279 = EDGE_LOOP('',(#10303,#10304,#10305)) ;
#4280 = EDGE_LOOP('',(#10306,#10307,#10308,#10309)) ;
#4281 = EDGE_LOOP('',(#10310,#10311,#10312)) ;
#4282 = EDGE_LOOP('',(#10313,#10314,#10315,#10316)) ;
#4283 = EDGE_LOOP('',(#10317,#10318,#10319)) ;
#4284 = EDGE_LOOP('',(#10320)) ;
#4285 = EDGE_LOOP('',(#10321)) ;
#4286 = EDGE_LOOP('',(#10322)) ;
#4287 = EDGE_LOOP('',(#10323)) ;
#4288 = EDGE_LOOP('',(#10324,#10325,#10326,#10327)) ;
#4289 = EDGE_LOOP('',(#10328)) ;
#4290 = EDGE_LOOP('',(#10329,#10330,#10331)) ;
#4291 = EDGE_LOOP('',(#10332)) ;
#4292 = EDGE_LOOP('',(#10333)) ;
#4293 = EDGE_LOOP('',(#10334)) ;
#4294 = EDGE_LOOP('',(#10335)) ;
#4295 = EDGE_LOOP('',(#10336)) ;
#4296 = EDGE_LOOP('',(#10337)) ;
#4297 = EDGE_LOOP('',(#10338,#10339,#10340,#10341,#10342,#10343)) ;
#4298 = EDGE_LOOP('',(#10344)) ;
#4299 = EDGE_LOOP('',(#10345,#10346)) ;
#4300 = EDGE_LOOP('',(#10347,#10348,#10349,#10350,#10351,#10352)) ;
#4301 = EDGE_LOOP('',(#10353)) ;
#4302 = EDGE_LOOP('',(#10354,#10355)) ;
#4303 = EDGE_LOOP('',(#10356)) ;
#4304 = EDGE_LOOP('',(#10357)) ;
#4305 = EDGE_LOOP('',(#10358)) ;
#4306 = EDGE_LOOP('',(#10359,#10360)) ;
#4307 = EDGE_LOOP('',(#10361,#10362)) ;
#4308 = EDGE_LOOP('',(#10363,#10364)) ;
#4309 = EDGE_LOOP('',(#10365)) ;
#4310 = EDGE_LOOP('',(#10366)) ;
#4311 = EDGE_LOOP('',(#10367,#10368)) ;
#4312 = EDGE_LOOP('',(#10369,#10370,#10371,#10372,#10373,#10374)) ;
#4313 = EDGE_LOOP('',(#10375,#10376)) ;
#4314 = EDGE_LOOP('',(#10377,#10378,#10379,#10380,#10381,#10382)) ;
#4315 = EDGE_LOOP('',(#10383,#10384)) ;
#4316 = EDGE_LOOP('',(#10385,#10386)) ;
#4317 = EDGE_LOOP('',(#10387,#10388)) ;
#4318 = EDGE_LOOP('',(#10389,#10390,#10391,#10392)) ;
#4319 = EDGE_LOOP('',(#10393,#10394,#10395,#10396)) ;
#4320 = EDGE_LOOP('',(#10397,#10398,#10399,#10400)) ;
#4321 = EDGE_LOOP('',(#10401,#10402,#10403,#10404)) ;
#4322 = EDGE_LOOP('',(#10405,#10406,#10407,#10408)) ;
#4323 = EDGE_LOOP('',(#10409,#10410,#10411,#10412)) ;
#4324 = EDGE_LOOP('',(#10413,#10414)) ;
#4325 = EDGE_LOOP('',(#10415,#10416,#10417,#10418,#10419)) ;
#4326 = EDGE_LOOP('',(#10420,#10421,#10422,#10423,#10424,#10425)) ;
#4327 = EDGE_LOOP('',(#10426,#10427,#10428,#10429,#10430,#10431,#10432)) ;
#4328 = EDGE_LOOP('',(#10433)) ;
#4329 = EDGE_LOOP('',(#10434)) ;
#4330 = EDGE_LOOP('',(#10435,#10436,#10437,#10438,#10439,#10440,#10441,#10442)) ;
#4331 = EDGE_LOOP('',(#10443,#10444,#10445)) ;
#4332 = EDGE_LOOP('',(#10446,#10447,#10448,#10449,#10450,#10451,#10452,#10453,
#10454)) ;
#4333 = EDGE_LOOP('',(#10455,#10456,#10457,#10458,#10459,#10460,#10461,#10462)) ;
#4334 = EDGE_LOOP('',(#10463,#10464,#10465,#10466,#10467,#10468,#10469,#10470)) ;
#4335 = EDGE_LOOP('',(#10471,#10472,#10473,#10474,#10475,#10476,#10477,#10478)) ;
#4336 = EDGE_LOOP('',(#10479,#10480,#10481,#10482,#10483,#10484,#10485,#10486)) ;
#4337 = EDGE_LOOP('',(#10487,#10488,#10489,#10490,#10491,#10492,#10493,#10494)) ;
#4338 = EDGE_LOOP('',(#10495,#10496,#10497,#10498,#10499,#10500,#10501,#10502)) ;
#4339 = EDGE_LOOP('',(#10503,#10504,#10505,#10506,#10507,#10508,#10509,#10510)) ;
#4340 = EDGE_LOOP('',(#10511,#10512,#10513,#10514,#10515,#10516,#10517,#10518)) ;
#4341 = EDGE_LOOP('',(#10519,#10520,#10521,#10522,#10523,#10524,#10525,#10526)) ;
#4342 = EDGE_LOOP('',(#10527,#10528,#10529,#10530,#10531,#10532,#10533,#10534)) ;
#4343 = EDGE_LOOP('',(#10535,#10536,#10537,#10538,#10539,#10540,#10541,#10542)) ;
#4344 = EDGE_LOOP('',(#10543,#10544,#10545,#10546,#10547,#10548,#10549,#10550,
#10551)) ;
#4345 = EDGE_LOOP('',(#10552,#10553,#10554)) ;
#4346 = EDGE_LOOP('',(#10555,#10556,#10557,#10558,#10559,#10560)) ;
#4347 = EDGE_LOOP('',(#10561)) ;
#4348 = EDGE_LOOP('',(#10562)) ;
#4349 = EDGE_LOOP('',(#10563,#10564,#10565,#10566)) ;
#4350 = EDGE_LOOP('',(#10567,#10568,#10569,#10570)) ;
#4351 = EDGE_LOOP('',(#10571,#10572,#10573,#10574)) ;
#4352 = EDGE_LOOP('',(#10575,#10576,#10577,#10578)) ;
#4353 = EDGE_LOOP('',(#10579,#10580,#10581,#10582)) ;
#4354 = EDGE_LOOP('',(#10583,#10584,#10585,#10586)) ;
#4355 = EDGE_LOOP('',(#10587,#10588,#10589,#10590,#10591)) ;
#4356 = EDGE_LOOP('',(#10592,#10593,#10594,#10595,#10596,#10597)) ;
#4357 = EDGE_LOOP('',(#10598,#10599,#10600,#10601,#10602)) ;
#4358 = EDGE_LOOP('',(#10603,#10604)) ;
#4359 = EDGE_LOOP('',(#10605)) ;
#4360 = EDGE_LOOP('',(#10606)) ;
#4361 = EDGE_LOOP('',(#10607)) ;
#4362 = EDGE_LOOP('',(#10608)) ;
#4363 = EDGE_LOOP('',(#10609,#10610,#10611)) ;
#4364 = EDGE_LOOP('',(#10612,#10613,#10614)) ;
#4365 = EDGE_LOOP('',(#10615,#10616,#10617)) ;
#4366 = EDGE_LOOP('',(#10618,#10619,#10620)) ;
#4367 = EDGE_LOOP('',(#10621,#10622,#10623)) ;
#4368 = EDGE_LOOP('',(#10624,#10625,#10626)) ;
#4369 = EDGE_LOOP('',(#10627,#10628,#10629)) ;
#4370 = EDGE_LOOP('',(#10630,#10631,#10632)) ;
#4371 = EDGE_LOOP('',(#10633,#10634,#10635,#10636)) ;
#4372 = EDGE_LOOP('',(#10637,#10638,#10639,#10640)) ;
#4373 = EDGE_LOOP('',(#10641,#10642,#10643,#10644)) ;
#4374 = EDGE_LOOP('',(#10645,#10646,#10647,#10648)) ;
#4375 = EDGE_LOOP('',(#10649,#10650,#10651,#10652)) ;
#4376 = EDGE_LOOP('',(#10653,#10654,#10655,#10656)) ;
#4377 = EDGE_LOOP('',(#10657,#10658,#10659,#10660)) ;
#4378 = EDGE_LOOP('',(#10661,#10662,#10663,#10664)) ;
#4379 = EDGE_LOOP('',(#10665,#10666,#10667,#10668)) ;
#4380 = EDGE_LOOP('',(#10669,#10670,#10671,#10672)) ;
#4381 = EDGE_LOOP('',(#10673,#10674,#10675,#10676)) ;
#4382 = EDGE_LOOP('',(#10677,#10678,#10679,#10680)) ;
#4383 = EDGE_LOOP('',(#10681,#10682,#10683,#10684)) ;
#4384 = EDGE_LOOP('',(#10685,#10686,#10687,#10688)) ;
#4385 = EDGE_LOOP('',(#10689,#10690,#10691,#10692)) ;
#4386 = EDGE_LOOP('',(#10693)) ;
#4387 = EDGE_LOOP('',(#10694)) ;
#4388 = EDGE_LOOP('',(#10695,#10696,#10697,#10698,#10699,#10700)) ;
#4389 = EDGE_LOOP('',(#10701,#10702,#10703,#10704)) ;
#4390 = EDGE_LOOP('',(#10705,#10706,#10707,#10708)) ;
#4391 = EDGE_LOOP('',(#10709,#10710,#10711,#10712)) ;
#4392 = EDGE_LOOP('',(#10713,#10714,#10715,#10716)) ;
#4393 = EDGE_LOOP('',(#10717,#10718,#10719,#10720)) ;
#4394 = EDGE_LOOP('',(#10721)) ;
#4395 = EDGE_LOOP('',(#10722)) ;
#4396 = EDGE_LOOP('',(#10723,#10724,#10725,#10726,#10727,#10728)) ;
#4397 = EDGE_LOOP('',(#10729,#10730,#10731,#10732,#10733,#10734)) ;
#4398 = EDGE_LOOP('',(#10735,#10736,#10737,#10738,#10739,#10740)) ;
#4399 = EDGE_LOOP('',(#10741,#10742,#10743,#10744,#10745,#10746)) ;
#4400 = EDGE_LOOP('',(#10747,#10748,#10749,#10750,#10751,#10752)) ;
#4401 = EDGE_LOOP('',(#10753,#10754,#10755,#10756)) ;
#4402 = EDGE_LOOP('',(#10757,#10758,#10759,#10760)) ;
#4403 = EDGE_LOOP('',(#10761,#10762,#10763,#10764)) ;
#4404 = EDGE_LOOP('',(#10765,#10766,#10767,#10768)) ;
#4405 = EDGE_LOOP('',(#10769,#10770,#10771,#10772)) ;
#4406 = EDGE_LOOP('',(#10773,#10774,#10775,#10776)) ;
#4407 = EDGE_LOOP('',(#10777,#10778,#10779,#10780)) ;
#4408 = EDGE_LOOP('',(#10781,#10782,#10783,#10784)) ;
#4409 = EDGE_LOOP('',(#10785,#10786,#10787,#10788)) ;
#4410 = EDGE_LOOP('',(#10789)) ;
#4411 = EDGE_LOOP('',(#10790,#10791,#10792,#10793)) ;
#4412 = EDGE_LOOP('',(#10794,#10795,#10796,#10797)) ;
#4413 = EDGE_LOOP('',(#10798,#10799,#10800,#10801)) ;
#4414 = EDGE_LOOP('',(#10802,#10803,#10804,#10805)) ;
#4415 = EDGE_LOOP('',(#10806,#10807,#10808,#10809)) ;
#4416 = EDGE_LOOP('',(#10810,#10811,#10812,#10813)) ;
#4417 = EDGE_LOOP('',(#10814,#10815,#10816,#10817)) ;
#4418 = EDGE_LOOP('',(#10818,#10819,#10820,#10821)) ;
#4419 = EDGE_LOOP('',(#10822,#10823,#10824,#10825)) ;
#4420 = EDGE_LOOP('',(#10826,#10827,#10828,#10829)) ;
#4421 = EDGE_LOOP('',(#10830,#10831,#10832,#10833)) ;
#4422 = EDGE_LOOP('',(#10834,#10835,#10836,#10837)) ;
#4423 = EDGE_LOOP('',(#10838)) ;
#4424 = EDGE_LOOP('',(#10839,#10840,#10841,#10842)) ;
#4425 = EDGE_LOOP('',(#10843,#10844,#10845,#10846)) ;
#4426 = EDGE_LOOP('',(#10847,#10848,#10849,#10850)) ;
#4427 = EDGE_LOOP('',(#10851,#10852,#10853,#10854)) ;
#4428 = EDGE_LOOP('',(#10855,#10856,#10857,#10858)) ;
#4429 = EDGE_LOOP('',(#10859,#10860,#10861,#10862)) ;
#4430 = EDGE_LOOP('',(#10863,#10864,#10865,#10866,#10867,#10868,#10869,#10870)) ;
#4431 = EDGE_LOOP('',(#10871,#10872,#10873,#10874)) ;
#4432 = EDGE_LOOP('',(#10875,#10876,#10877,#10878,#10879,#10880)) ;
#4433 = EDGE_LOOP('',(#10881,#10882,#10883,#10884,#10885,#10886)) ;
#4434 = EDGE_LOOP('',(#10887,#10888,#10889,#10890,#10891,#10892)) ;
#4435 = EDGE_LOOP('',(#10893,#10894,#10895)) ;
#4436 = EDGE_LOOP('',(#10896,#10897,#10898)) ;
#4437 = EDGE_LOOP('',(#10899,#10900,#10901)) ;
#4438 = EDGE_LOOP('',(#10902,#10903,#10904)) ;
#4439 = EDGE_LOOP('',(#10905,#10906,#10907,#10908)) ;
#4440 = EDGE_LOOP('',(#10909,#10910,#10911,#10912,#10913,#10914)) ;
#4441 = EDGE_LOOP('',(#10915,#10916,#10917,#10918,#10919,#10920,#10921,#10922)) ;
#4442 = EDGE_LOOP('',(#10923,#10924,#10925)) ;
#4443 = EDGE_LOOP('',(#10926,#10927,#10928)) ;
#4444 = EDGE_LOOP('',(#10929,#10930,#10931)) ;
#4445 = EDGE_LOOP('',(#10932,#10933,#10934)) ;
#4446 = EDGE_LOOP('',(#10935,#10936)) ;
#4447 = EDGE_LOOP('',(#10937,#10938,#10939,#10940,#10941)) ;
#4448 = EDGE_LOOP('',(#10942,#10943,#10944,#10945)) ;
#4449 = EDGE_LOOP('',(#10946,#10947,#10948,#10949)) ;
#4450 = EDGE_LOOP('',(#10950,#10951,#10952,#10953)) ;
#4451 = EDGE_LOOP('',(#10954,#10955,#10956,#10957,#10958,#10959,#10960,#10961,
#10962,#10963,#10964,#10965)) ;
#4452 = EDGE_LOOP('',(#10966,#10967)) ;
#4453 = EDGE_LOOP('',(#10968)) ;
#4454 = EDGE_LOOP('',(#10969)) ;
#4455 = EDGE_LOOP('',(#10970)) ;
#4456 = EDGE_LOOP('',(#10971)) ;
#4457 = EDGE_LOOP('',(#10972,#10973,#10974)) ;
#4458 = EDGE_LOOP('',(#10975,#10976,#10977,#10978,#10979,#10980,#10981,#10982,
#10983,#10984,#10985,#10986,#10987,#10988,#10989,#10990,#10991,#10992,#10993,
#10994,#10995,#10996,#10997,#10998)) ;
#4459 = EDGE_LOOP('',(#10999,#11000,#11001,#11002)) ;
#4460 = EDGE_LOOP('',(#11003)) ;
#4461 = EDGE_LOOP('',(#11004,#11005,#11006,#11007)) ;
#4462 = EDGE_LOOP('',(#11008)) ;
#4463 = EDGE_LOOP('',(#11009,#11010,#11011,#11012)) ;
#4464 = EDGE_LOOP('',(#11013)) ;
#4465 = EDGE_LOOP('',(#11014,#11015,#11016,#11017)) ;
#4466 = EDGE_LOOP('',(#11018,#11019,#11020,#11021)) ;
#4467 = EDGE_LOOP('',(#11022)) ;
#4468 = EDGE_LOOP('',(#11023,#11024,#11025,#11026)) ;
#4469 = EDGE_LOOP('',(#11027,#11028,#11029,#11030)) ;
#4470 = EDGE_LOOP('',(#11031,#11032,#11033,#11034)) ;
#4471 = EDGE_LOOP('',(#11035,#11036,#11037,#11038,#11039,#11040,#11041,#11042,
#11043,#11044,#11045,#11046,#11047,#11048,#11049,#11050)) ;
#4472 = EDGE_LOOP('',(#11051)) ;
#4473 = EDGE_LOOP('',(#11052,#11053,#11054,#11055)) ;
#4474 = EDGE_LOOP('',(#11056,#11057,#11058,#11059)) ;
#4475 = EDGE_LOOP('',(#11060,#11061,#11062,#11063)) ;
#4476 = EDGE_LOOP('',(#11064,#11065,#11066,#11067)) ;
#4477 = EDGE_LOOP('',(#11068,#11069,#11070,#11071)) ;
#4478 = EDGE_LOOP('',(#11072,#11073,#11074,#11075)) ;
#4479 = EDGE_LOOP('',(#11076,#11077,#11078,#11079)) ;
#4480 = EDGE_LOOP('',(#11080,#11081,#11082,#11083)) ;
#4481 = EDGE_LOOP('',(#11084,#11085,#11086,#11087)) ;
#4482 = EDGE_LOOP('',(#11088,#11089,#11090,#11091)) ;
#4483 = EDGE_LOOP('',(#11092,#11093,#11094,#11095)) ;
#4484 = EDGE_LOOP('',(#11096,#11097,#11098,#11099)) ;
#4485 = EDGE_LOOP('',(#11100,#11101,#11102,#11103)) ;
#4486 = EDGE_LOOP('',(#11104,#11105,#11106,#11107)) ;
#4487 = EDGE_LOOP('',(#11108,#11109,#11110,#11111,#11112,#11113,#11114,#11115,
#11116,#11117,#11118,#11119,#11120,#11121,#11122,#11123)) ;
#4488 = EDGE_LOOP('',(#11124)) ;
#4489 = EDGE_LOOP('',(#11125,#11126,#11127,#11128)) ;
#4490 = EDGE_LOOP('',(#11129,#11130,#11131,#11132)) ;
#4491 = EDGE_LOOP('',(#11133)) ;
#4492 = EDGE_LOOP('',(#11134)) ;
#4493 = EDGE_LOOP('',(#11135,#11136,#11137,#11138)) ;
#4494 = EDGE_LOOP('',(#11139,#11140,#11141,#11142)) ;
#4495 = EDGE_LOOP('',(#11143)) ;
#4496 = EDGE_LOOP('',(#11144)) ;
#4497 = EDGE_LOOP('',(#11145)) ;
#4498 = EDGE_LOOP('',(#11146)) ;
#4499 = EDGE_LOOP('',(#11147,#11148,#11149,#11150)) ;
#4500 = EDGE_LOOP('',(#11151,#11152,#11153,#11154)) ;
#4501 = EDGE_LOOP('',(#11155)) ;
#4502 = EDGE_LOOP('',(#11156)) ;
#4503 = EDGE_LOOP('',(#11157,#11158,#11159,#11160)) ;
#4504 = EDGE_LOOP('',(#11161,#11162,#11163,#11164)) ;
#4505 = EDGE_LOOP('',(#11165,#11166,#11167,#11168)) ;
#4506 = EDGE_LOOP('',(#11169,#11170,#11171,#11172)) ;
#4507 = EDGE_LOOP('',(#11173,#11174,#11175,#11176)) ;
#4508 = EDGE_LOOP('',(#11177,#11178,#11179,#11180)) ;
#4509 = EDGE_LOOP('',(#11181,#11182,#11183,#11184)) ;
#4510 = EDGE_LOOP('',(#11185,#11186,#11187,#11188)) ;
#4511 = EDGE_LOOP('',(#11189,#11190,#11191,#11192)) ;
#4512 = EDGE_LOOP('',(#11193,#11194,#11195,#11196)) ;
#4513 = EDGE_LOOP('',(#11197,#11198,#11199,#11200)) ;
#4514 = EDGE_LOOP('',(#11201,#11202,#11203,#11204)) ;
#4515 = EDGE_LOOP('',(#11205,#11206,#11207,#11208)) ;
#4516 = EDGE_LOOP('',(#11209,#11210,#11211,#11212)) ;
#4517 = EDGE_LOOP('',(#11213,#11214,#11215,#11216)) ;
#4518 = EDGE_LOOP('',(#11217,#11218,#11219,#11220)) ;
#4519 = EDGE_LOOP('',(#11221,#11222,#11223,#11224)) ;
#4520 = EDGE_LOOP('',(#11225,#11226,#11227,#11228)) ;
#4521 = EDGE_LOOP('',(#11229,#11230,#11231,#11232)) ;
#4522 = EDGE_LOOP('',(#11233,#11234,#11235,#11236)) ;
#4523 = EDGE_LOOP('',(#11237,#11238,#11239,#11240,#11241)) ;
#4524 = EDGE_LOOP('',(#11242,#11243,#11244,#11245)) ;
#4525 = EDGE_LOOP('',(#11246,#11247,#11248,#11249)) ;
#4526 = EDGE_LOOP('',(#11250,#11251,#11252,#11253,#11254)) ;
#4527 = EDGE_LOOP('',(#11255,#11256,#11257,#11258)) ;
#4528 = EDGE_LOOP('',(#11259,#11260,#11261,#11262)) ;
#4529 = EDGE_LOOP('',(#11263,#11264,#11265,#11266)) ;
#4530 = EDGE_LOOP('',(#11267,#11268,#11269,#11270)) ;
#4531 = EDGE_LOOP('',(#11271,#11272,#11273,#11274)) ;
#4532 = EDGE_LOOP('',(#11275,#11276,#11277,#11278)) ;
#4533 = EDGE_LOOP('',(#11279,#11280,#11281,#11282)) ;
#4534 = EDGE_LOOP('',(#11283,#11284,#11285,#11286)) ;
#4535 = EDGE_LOOP('',(#11287,#11288,#11289,#11290)) ;
#4536 = EDGE_LOOP('',(#11291,#11292,#11293,#11294)) ;
#4537 = EDGE_LOOP('',(#11295,#11296,#11297,#11298)) ;
#4538 = EDGE_LOOP('',(#11299,#11300,#11301,#11302)) ;
#4539 = EDGE_LOOP('',(#11303,#11304,#11305,#11306)) ;
#4540 = EDGE_LOOP('',(#11307,#11308,#11309,#11310)) ;
#4541 = EDGE_LOOP('',(#11311,#11312,#11313,#11314)) ;
#4542 = EDGE_LOOP('',(#11315,#11316,#11317,#11318)) ;
#4543 = EDGE_LOOP('',(#11319,#11320,#11321,#11322)) ;
#4544 = EDGE_LOOP('',(#11323,#11324,#11325,#11326)) ;
#4545 = EDGE_LOOP('',(#11327,#11328,#11329,#11330)) ;
#4546 = EDGE_LOOP('',(#11331,#11332,#11333,#11334)) ;
#4547 = EDGE_LOOP('',(#11335,#11336,#11337,#11338)) ;
#4548 = EDGE_LOOP('',(#11339,#11340,#11341,#11342)) ;
#4549 = EDGE_LOOP('',(#11343,#11344,#11345,#11346)) ;
#4550 = EDGE_LOOP('',(#11347,#11348,#11349,#11350)) ;
#4551 = EDGE_LOOP('',(#11351,#11352,#11353,#11354)) ;
#4552 = EDGE_LOOP('',(#11355,#11356,#11357,#11358)) ;
#4553 = EDGE_LOOP('',(#11359,#11360,#11361,#11362,#11363,#11364,#11365,#11366,
#11367,#11368,#11369,#11370)) ;
#4554 = EDGE_LOOP('',(#11371,#11372,#11373,#11374)) ;
#4555 = EDGE_LOOP('',(#11375,#11376,#11377,#11378)) ;
#4556 = EDGE_LOOP('',(#11379,#11380,#11381,#11382)) ;
#4557 = EDGE_LOOP('',(#11383,#11384,#11385,#11386)) ;
#4558 = EDGE_LOOP('',(#11387,#11388,#11389,#11390)) ;
#4559 = EDGE_LOOP('',(#11391,#11392,#11393,#11394)) ;
#4560 = EDGE_LOOP('',(#11395,#11396,#11397,#11398)) ;
#4561 = EDGE_LOOP('',(#11399,#11400,#11401,#11402)) ;
#4562 = EDGE_LOOP('',(#11403,#11404,#11405,#11406)) ;
#4563 = EDGE_LOOP('',(#11407)) ;
#4564 = EDGE_LOOP('',(#11408)) ;
#4565 = EDGE_LOOP('',(#11409)) ;
#4566 = EDGE_LOOP('',(#11410)) ;
#4567 = EDGE_LOOP('',(#11411,#11412,#11413,#11414)) ;
#4568 = EDGE_LOOP('',(#11415,#11416,#11417,#11418)) ;
#4569 = EDGE_LOOP('',(#11419)) ;
#4570 = EDGE_LOOP('',(#11420)) ;
#4571 = EDGE_LOOP('',(#11421)) ;
#4572 = EDGE_LOOP('',(#11422)) ;
#4573 = EDGE_LOOP('',(#11423,#11424,#11425,#11426)) ;
#4574 = EDGE_LOOP('',(#11427,#11428,#11429,#11430,#11431)) ;
#4575 = EDGE_LOOP('',(#11432,#11433,#11434,#11435,#11436,#11437,#11438)) ;
#4576 = EDGE_LOOP('',(#11439)) ;
#4577 = EDGE_LOOP('',(#11440)) ;
#4578 = EDGE_LOOP('',(#11441,#11442,#11443,#11444,#11445,#11446,#11447)) ;
#4579 = EDGE_LOOP('',(#11448,#11449)) ;
#4580 = EDGE_LOOP('',(#11450)) ;
#4581 = EDGE_LOOP('',(#11451,#11452)) ;
#4582 = EDGE_LOOP('',(#11453,#11454,#11455,#11456,#11457,#11458)) ;
#4583 = EDGE_LOOP('',(#11459,#11460)) ;
#4584 = EDGE_LOOP('',(#11461,#11462,#11463,#11464,#11465,#11466)) ;
#4585 = EDGE_LOOP('',(#11467,#11468,#11469,#11470,#11471,#11472,#11473,#11474,
#11475)) ;
#4586 = EDGE_LOOP('',(#11476,#11477,#11478,#11479,#11480,#11481,#11482,#11483)) ;
#4587 = EDGE_LOOP('',(#11484,#11485,#11486,#11487)) ;
#4588 = EDGE_LOOP('',(#11488,#11489,#11490,#11491,#11492)) ;
#4589 = EDGE_LOOP('',(#11493)) ;
#4590 = EDGE_LOOP('',(#11494)) ;
#4591 = EDGE_LOOP('',(#11495,#11496,#11497,#11498)) ;
#4592 = EDGE_LOOP('',(#11499,#11500,#11501,#11502)) ;
#4593 = EDGE_LOOP('',(#11503,#11504,#11505,#11506)) ;
#4594 = EDGE_LOOP('',(#11507,#11508,#11509,#11510)) ;
#4595 = EDGE_LOOP('',(#11511,#11512,#11513,#11514)) ;
#4596 = EDGE_LOOP('',(#11515,#11516)) ;
#4597 = EDGE_LOOP('',(#11517,#11518,#11519,#11520)) ;
#4598 = EDGE_LOOP('',(#11521,#11522,#11523,#11524)) ;
#4599 = EDGE_LOOP('',(#11525,#11526,#11527,#11528)) ;
#4600 = EDGE_LOOP('',(#11529,#11530)) ;
#4601 = EDGE_LOOP('',(#11531,#11532,#11533,#11534)) ;
#4602 = EDGE_LOOP('',(#11535,#11536,#11537,#11538)) ;
#4603 = EDGE_LOOP('',(#11539,#11540,#11541,#11542)) ;
#4604 = EDGE_LOOP('',(#11543,#11544,#11545,#11546)) ;
#4605 = EDGE_LOOP('',(#11547,#11548,#11549,#11550)) ;
#4606 = EDGE_LOOP('',(#11551,#11552,#11553,#11554)) ;
#4607 = EDGE_LOOP('',(#11555,#11556,#11557,#11558)) ;
#4608 = EDGE_LOOP('',(#11559,#11560)) ;
#4609 = EDGE_LOOP('',(#11561,#11562,#11563,#11564)) ;
#4610 = EDGE_LOOP('',(#11565,#11566)) ;
#4611 = EDGE_LOOP('',(#11567,#11568,#11569,#11570,#11571,#11572,#11573,#11574)) ;
#4612 = EDGE_LOOP('',(#11575,#11576,#11577,#11578,#11579,#11580,#11581,#11582,
#11583)) ;
#4613 = EDGE_LOOP('',(#11584,#11585,#11586,#11587,#11588,#11589,#11590,#11591,
#11592)) ;
#4614 = EDGE_LOOP('',(#11593)) ;
#4615 = EDGE_LOOP('',(#11594)) ;
#4616 = EDGE_LOOP('',(#11595)) ;
#4617 = EDGE_LOOP('',(#11596)) ;
#4618 = EDGE_LOOP('',(#11597,#11598,#11599,#11600)) ;
#4619 = EDGE_LOOP('',(#11601,#11602,#11603,#11604,#11605,#11606)) ;
#4620 = EDGE_LOOP('',(#11607,#11608,#11609,#11610,#11611,#11612)) ;
#4621 = EDGE_LOOP('',(#11613,#11614,#11615,#11616)) ;
#4622 = EDGE_LOOP('',(#11617,#11618,#11619,#11620,#11621,#11622,#11623,#11624,
#11625,#11626,#11627,#11628)) ;
#4623 = EDGE_LOOP('',(#11629,#11630,#11631,#11632)) ;
#4624 = EDGE_LOOP('',(#11633)) ;
#4625 = EDGE_LOOP('',(#11634)) ;
#4626 = EDGE_LOOP('',(#11635,#11636,#11637,#11638,#11639,#11640,#11641,#11642,
#11643,#11644,#11645,#11646)) ;
#4627 = EDGE_LOOP('',(#11647,#11648,#11649,#11650)) ;
#4628 = EDGE_LOOP('',(#11651)) ;
#4629 = EDGE_LOOP('',(#11652)) ;
#4630 = EDGE_LOOP('',(#11653,#11654,#11655,#11656)) ;
#4631 = EDGE_LOOP('',(#11657,#11658,#11659,#11660)) ;
#4632 = EDGE_LOOP('',(#11661)) ;
#4633 = EDGE_LOOP('',(#11662)) ;
#4634 = EDGE_LOOP('',(#11663)) ;
#4635 = EDGE_LOOP('',(#11664)) ;
#4636 = EDGE_LOOP('',(#11665,#11666,#11667,#11668)) ;
#4637 = EDGE_LOOP('',(#11669,#11670,#11671,#11672)) ;
#4638 = EDGE_LOOP('',(#11673,#11674,#11675,#11676)) ;
#4639 = EDGE_LOOP('',(#11677,#11678,#11679,#11680)) ;
#4640 = EDGE_LOOP('',(#11681,#11682,#11683,#11684)) ;
#4641 = EDGE_LOOP('',(#11685,#11686,#11687,#11688)) ;
#4642 = EDGE_LOOP('',(#11689)) ;
#4643 = EDGE_LOOP('',(#11690)) ;
#4644 = EDGE_LOOP('',(#11691)) ;
#4645 = EDGE_LOOP('',(#11692)) ;
#4646 = EDGE_LOOP('',(#11693)) ;
#4647 = EDGE_LOOP('',(#11694)) ;
#4648 = EDGE_LOOP('',(#11695)) ;
#4649 = EDGE_LOOP('',(#11696)) ;
#4650 = EDGE_LOOP('',(#11697)) ;
#4651 = EDGE_LOOP('',(#11698)) ;
#4652 = EDGE_LOOP('',(#11699)) ;
#4653 = EDGE_LOOP('',(#11700)) ;
#4654 = EDGE_LOOP('',(#11701,#11702,#11703,#11704)) ;
#4655 = EDGE_LOOP('',(#11705,#11706,#11707,#11708)) ;
#4656 = EDGE_LOOP('',(#11709,#11710,#11711,#11712)) ;
#4657 = EDGE_LOOP('',(#11713,#11714,#11715,#11716)) ;
#4658 = EDGE_LOOP('',(#11717,#11718,#11719,#11720)) ;
#4659 = EDGE_LOOP('',(#11721,#11722,#11723,#11724)) ;
#4660 = EDGE_LOOP('',(#11725)) ;
#4661 = EDGE_LOOP('',(#11726)) ;
#4662 = EDGE_LOOP('',(#11727)) ;
#4663 = EDGE_LOOP('',(#11728)) ;
#4664 = EDGE_LOOP('',(#11729)) ;
#4665 = EDGE_LOOP('',(#11730)) ;
#4666 = EDGE_LOOP('',(#11731)) ;
#4667 = EDGE_LOOP('',(#11732)) ;
#4668 = EDGE_LOOP('',(#11733)) ;
#4669 = EDGE_LOOP('',(#11734)) ;
#4670 = EDGE_LOOP('',(#11735)) ;
#4671 = EDGE_LOOP('',(#11736)) ;
#4672 = EDGE_LOOP('',(#11737,#11738)) ;
#4673 = EDGE_LOOP('',(#11739,#11740,#11741,#11742)) ;
#4674 = EDGE_LOOP('',(#11743,#11744)) ;
#4675 = EDGE_LOOP('',(#11745,#11746)) ;
#4676 = EDGE_LOOP('',(#11747,#11748,#11749,#11750)) ;
#4677 = EDGE_LOOP('',(#11751,#11752)) ;
#4678 = EDGE_LOOP('',(#11753,#11754,#11755,#11756)) ;
#4679 = EDGE_LOOP('',(#11757)) ;
#4680 = EDGE_LOOP('',(#11758,#11759,#11760,#11761)) ;
#4681 = EDGE_LOOP('',(#11762)) ;
#4682 = EDGE_LOOP('',(#11763,#11764,#11765,#11766)) ;
#4683 = EDGE_LOOP('',(#11767)) ;
#4684 = EDGE_LOOP('',(#11768)) ;
#4685 = EDGE_LOOP('',(#11769,#11770,#11771,#11772)) ;
#4686 = EDGE_LOOP('',(#11773,#11774,#11775,#11776)) ;
#4687 = EDGE_LOOP('',(#11777,#11778,#11779,#11780,#11781,#11782)) ;
#4688 = EDGE_LOOP('',(#11783)) ;
#4689 = EDGE_LOOP('',(#11784,#11785,#11786,#11787)) ;
#4690 = EDGE_LOOP('',(#11788,#11789)) ;
#4691 = EDGE_LOOP('',(#11790,#11791)) ;
#4692 = EDGE_LOOP('',(#11792,#11793,#11794,#11795)) ;
#4693 = EDGE_LOOP('',(#11796,#11797,#11798,#11799,#11800,#11801)) ;
#4694 = EDGE_LOOP('',(#11802)) ;
#4695 = EDGE_LOOP('',(#11803,#11804,#11805,#11806)) ;
#4696 = EDGE_LOOP('',(#11807)) ;
#4697 = EDGE_LOOP('',(#11808,#11809,#11810,#11811)) ;
#4698 = EDGE_LOOP('',(#11812)) ;
#4699 = EDGE_LOOP('',(#11813)) ;
#4700 = EDGE_LOOP('',(#11814)) ;
#4701 = EDGE_LOOP('',(#11815,#11816,#11817,#11818)) ;
#4702 = EDGE_LOOP('',(#11819,#11820,#11821,#11822)) ;
#4703 = EDGE_LOOP('',(#11823)) ;
#4704 = EDGE_LOOP('',(#11824)) ;
#4705 = EDGE_LOOP('',(#11825)) ;
#4706 = EDGE_LOOP('',(#11826)) ;
#4707 = EDGE_LOOP('',(#11827,#11828,#11829,#11830)) ;
#4708 = EDGE_LOOP('',(#11831,#11832,#11833,#11834)) ;
#4709 = EDGE_LOOP('',(#11835,#11836,#11837,#11838)) ;
#4710 = EDGE_LOOP('',(#11839,#11840,#11841,#11842,#11843,#11844)) ;
#4711 = EDGE_LOOP('',(#11845)) ;
#4712 = EDGE_LOOP('',(#11846,#11847,#11848,#11849)) ;
#4713 = EDGE_LOOP('',(#11850,#11851,#11852,#11853)) ;
#4714 = EDGE_LOOP('',(#11854,#11855,#11856,#11857)) ;
#4715 = EDGE_LOOP('',(#11858,#11859,#11860,#11861)) ;
#4716 = EDGE_LOOP('',(#11862,#11863,#11864,#11865,#11866,#11867)) ;
#4717 = EDGE_LOOP('',(#11868)) ;
#4718 = EDGE_LOOP('',(#11869,#11870,#11871,#11872)) ;
#4719 = EDGE_LOOP('',(#11873)) ;
#4720 = EDGE_LOOP('',(#11874,#11875,#11876,#11877)) ;
#4721 = EDGE_LOOP('',(#11878,#11879,#11880,#11881)) ;
#4722 = EDGE_LOOP('',(#11882,#11883,#11884,#11885,#11886,#11887)) ;
#4723 = EDGE_LOOP('',(#11888,#11889,#11890,#11891)) ;
#4724 = EDGE_LOOP('',(#11892,#11893,#11894,#11895)) ;
#4725 = EDGE_LOOP('',(#11896,#11897,#11898,#11899)) ;
#4726 = EDGE_LOOP('',(#11900,#11901,#11902,#11903)) ;
#4727 = EDGE_LOOP('',(#11904,#11905,#11906,#11907,#11908,#11909)) ;
#4728 = EDGE_LOOP('',(#11910)) ;
#4729 = EDGE_LOOP('',(#11911,#11912,#11913,#11914)) ;
#4730 = EDGE_LOOP('',(#11915)) ;
#4731 = EDGE_LOOP('',(#11916,#11917,#11918,#11919)) ;
#4732 = EDGE_LOOP('',(#11920,#11921,#11922,#11923)) ;
#4733 = EDGE_LOOP('',(#11924,#11925,#11926,#11927,#11928,#11929)) ;
#4734 = EDGE_LOOP('',(#11930,#11931,#11932,#11933)) ;
#4735 = EDGE_LOOP('',(#11934,#11935,#11936,#11937)) ;
#4736 = EDGE_LOOP('',(#11938,#11939,#11940,#11941)) ;
#4737 = EDGE_LOOP('',(#11942,#11943,#11944,#11945)) ;
#4738 = EDGE_LOOP('',(#11946,#11947,#11948,#11949,#11950,#11951)) ;
#4739 = EDGE_LOOP('',(#11952)) ;
#4740 = EDGE_LOOP('',(#11953,#11954,#11955,#11956)) ;
#4741 = EDGE_LOOP('',(#11957,#11958,#11959,#11960)) ;
#4742 = EDGE_LOOP('',(#11961,#11962,#11963,#11964)) ;
#4743 = EDGE_LOOP('',(#11965,#11966,#11967,#11968,#11969,#11970)) ;
#4744 = EDGE_LOOP('',(#11971)) ;
#4745 = EDGE_LOOP('',(#11972,#11973,#11974,#11975)) ;
#4746 = EDGE_LOOP('',(#11976,#11977,#11978,#11979)) ;
#4747 = EDGE_LOOP('',(#11980,#11981,#11982,#11983)) ;
#4748 = EDGE_LOOP('',(#11984,#11985,#11986,#11987)) ;
#4749 = EDGE_LOOP('',(#11988,#11989,#11990,#11991,#11992,#11993)) ;
#4750 = EDGE_LOOP('',(#11994)) ;
#4751 = CIRCLE('',#13656,11.4) ;
#4752 = CIRCLE('',#13657,0.41) ;
#4753 = CIRCLE('',#13658,0.41) ;
#4754 = CIRCLE('',#13660,0.41) ;
#4755 = CIRCLE('',#13661,0.41) ;
#4756 = CIRCLE('',#13663,11.4) ;
#4757 = CIRCLE('',#13664,11.4) ;
#4758 = CIRCLE('',#13665,11.4) ;
#4759 = CIRCLE('',#13666,11.4) ;
#4760 = CIRCLE('',#13667,11.4) ;
#4761 = CIRCLE('',#13668,11.4) ;
#4762 = CIRCLE('',#13669,11.4) ;
#4763 = CIRCLE('',#13671,0.41) ;
#4764 = CIRCLE('',#13672,0.41) ;
#4765 = CIRCLE('',#13673,0.41) ;
#4766 = CIRCLE('',#13674,0.41) ;
#4767 = CIRCLE('',#13677,0.9) ;
#4768 = CIRCLE('',#13678,0.9) ;
#4769 = CIRCLE('',#13679,2.5) ;
#4770 = CIRCLE('',#13681,0.325) ;
#4771 = CIRCLE('',#13682,0.325) ;
#4772 = CIRCLE('',#13684,0.325) ;
#4773 = CIRCLE('',#13685,0.325) ;
#4774 = CIRCLE('',#13687,0.325) ;
#4775 = CIRCLE('',#13688,0.325) ;
#4776 = CIRCLE('',#13690,0.325) ;
#4777 = CIRCLE('',#13691,0.325) ;
#4778 = CIRCLE('',#13693,0.325) ;
#4779 = CIRCLE('',#13694,0.325) ;
#4780 = CIRCLE('',#13696,0.325) ;
#4781 = CIRCLE('',#13697,0.325) ;
#4782 = CIRCLE('',#13701,12.5) ;
#4783 = CIRCLE('',#13705,12.5) ;
#4784 = CIRCLE('',#13708,12.5) ;
#4785 = CIRCLE('',#13709,12.5) ;
#4786 = CIRCLE('',#13710,12.5) ;
#4787 = CIRCLE('',#13711,12.5) ;
#4788 = CIRCLE('',#13712,12.5) ;
#4789 = CIRCLE('',#13714,1.1) ;
#4790 = CIRCLE('',#13715,1.1) ;
#4791 = CIRCLE('',#13717,1.5) ;
#4792 = CIRCLE('',#13719,1.5) ;
#4793 = CIRCLE('',#13723,0.9) ;
#4794 = CIRCLE('',#13725,0.9) ;
#4795 = CIRCLE('',#13727,1.2) ;
#4796 = CIRCLE('',#13729,1.2) ;
#4797 = CIRCLE('',#13730,1.2) ;
#4798 = CIRCLE('',#13731,1.2) ;
#4799 = CIRCLE('',#13734,2.5) ;
#4800 = CIRCLE('',#13736,1.5) ;
#4801 = CIRCLE('',#13737,1.5) ;
#4802 = CIRCLE('',#13739,1.75) ;
#4803 = CIRCLE('',#13740,1.75) ;
#4804 = CIRCLE('',#13743,1.75) ;
#4805 = CIRCLE('',#13744,1.75) ;
#4806 = CIRCLE('',#13747,2.5) ;
#4807 = CIRCLE('',#13750,2.5) ;
#4808 = CIRCLE('',#13755,0.2025) ;
#4809 = CIRCLE('',#13756,0.2025) ;
#4810 = CIRCLE('',#13758,0.325) ;
#4811 = CIRCLE('',#13759,0.325) ;
#4812 = CIRCLE('',#13761,0.325) ;
#4813 = CIRCLE('',#13762,0.325) ;
#4814 = CIRCLE('',#13764,0.325) ;
#4815 = CIRCLE('',#13765,0.325) ;
#4816 = CIRCLE('',#13767,0.325) ;
#4817 = CIRCLE('',#13768,0.325) ;
#4818 = CIRCLE('',#13770,0.325) ;
#4819 = CIRCLE('',#13771,0.325) ;
#4820 = CIRCLE('',#13773,0.325) ;
#4821 = CIRCLE('',#13774,0.325) ;
#4822 = CIRCLE('',#13776,1.41) ;
#4823 = CIRCLE('',#13777,1.41) ;
#4824 = CIRCLE('',#13779,1.8) ;
#4825 = CIRCLE('',#13780,1.8) ;
#4826 = CIRCLE('',#13783,1.41) ;
#4827 = CIRCLE('',#13784,1.41) ;
#4828 = CIRCLE('',#13786,1.8) ;
#4829 = CIRCLE('',#13787,1.8) ;
#4830 = CIRCLE('',#13790,5.9) ;
#4831 = CIRCLE('',#13791,5.9) ;
#4832 = CIRCLE('',#13793,5.5) ;
#4833 = CIRCLE('',#13795,5.5) ;
#4834 = CIRCLE('',#13797,11.4) ;
#4835 = CIRCLE('',#13798,11.4) ;
#4836 = CIRCLE('',#13801,12.5) ;
#4837 = CIRCLE('',#13802,12.5) ;
#4838 = CIRCLE('',#13807,5.89) ;
#4839 = CIRCLE('',#13808,5.89) ;
#4840 = CIRCLE('',#13813,0.325) ;
#4841 = CIRCLE('',#13814,0.325) ;
#4842 = CIRCLE('',#13816,0.325) ;
#4843 = CIRCLE('',#13817,0.325) ;
#4844 = CIRCLE('',#13819,0.325) ;
#4845 = CIRCLE('',#13820,0.325) ;
#4846 = CIRCLE('',#13822,0.325) ;
#4847 = CIRCLE('',#13823,0.325) ;
#4848 = CIRCLE('',#13825,0.325) ;
#4849 = CIRCLE('',#13826,0.325) ;
#4850 = CIRCLE('',#13828,0.325) ;
#4851 = CIRCLE('',#13829,0.325) ;
#4852 = CIRCLE('',#13831,11.4) ;
#4853 = CIRCLE('',#13832,11.4) ;
#4854 = CIRCLE('',#13834,12.5) ;
#4855 = CIRCLE('',#13835,12.5) ;
#4856 = CIRCLE('',#13841,0.75) ;
#4857 = CIRCLE('',#13845,0.75) ;
#4858 = CIRCLE('',#13846,0.75) ;
#4859 = CIRCLE('',#13847,0.75) ;
#4860 = CIRCLE('',#13849,0.7) ;
#4861 = CIRCLE('',#13850,0.7) ;
#4862 = CIRCLE('',#13853,0.75) ;
#4863 = CIRCLE('',#13855,0.75) ;
#4864 = CIRCLE('',#13857,0.195) ;
#4865 = CIRCLE('',#13858,0.195) ;
#4866 = CIRCLE('',#13860,0.195) ;
#4867 = CIRCLE('',#13861,0.195) ;
#4868 = CIRCLE('',#13863,0.195) ;
#4869 = CIRCLE('',#13864,0.195) ;
#4870 = CIRCLE('',#13866,2.5) ;
#4871 = CIRCLE('',#13868,2.5) ;
#4872 = CIRCLE('',#13870,0.5) ;
#4873 = CIRCLE('',#13871,0.5) ;
#4874 = CIRCLE('',#13877,0.15) ;
#4875 = CIRCLE('',#13878,0.15) ;
#4876 = CIRCLE('',#13881,0.15) ;
#4877 = CIRCLE('',#13882,0.15) ;
#4878 = CIRCLE('',#13885,0.15) ;
#4879 = CIRCLE('',#13886,0.15) ;
#4880 = CIRCLE('',#13889,0.15) ;
#4881 = CIRCLE('',#13890,0.15) ;
#4882 = CIRCLE('',#13893,0.15) ;
#4883 = CIRCLE('',#13894,0.15) ;
#4884 = CIRCLE('',#13897,0.15) ;
#4885 = CIRCLE('',#13898,0.15) ;
#4886 = CIRCLE('',#13901,0.15) ;
#4887 = CIRCLE('',#13902,0.15) ;
#4888 = CIRCLE('',#13905,0.15) ;
#4889 = CIRCLE('',#13906,0.15) ;
#4890 = CIRCLE('',#13909,0.15) ;
#4891 = CIRCLE('',#13910,0.15) ;
#4892 = CIRCLE('',#13913,0.15) ;
#4893 = CIRCLE('',#13914,0.15) ;
#4894 = CIRCLE('',#13917,0.15) ;
#4895 = CIRCLE('',#13918,0.15) ;
#4896 = CIRCLE('',#13921,0.15) ;
#4897 = CIRCLE('',#13922,0.15) ;
#4898 = CIRCLE('',#13925,0.15) ;
#4899 = CIRCLE('',#13926,0.15) ;
#4900 = CIRCLE('',#13929,0.15) ;
#4901 = CIRCLE('',#13930,0.15) ;
#4902 = CIRCLE('',#13933,0.15) ;
#4903 = CIRCLE('',#13934,0.15) ;
#4904 = CIRCLE('',#13937,0.15) ;
#4905 = CIRCLE('',#13938,0.15) ;
#4906 = CIRCLE('',#13941,0.15) ;
#4907 = CIRCLE('',#13942,0.15) ;
#4908 = CIRCLE('',#13945,0.15) ;
#4909 = CIRCLE('',#13946,0.15) ;
#4910 = CIRCLE('',#13949,0.15) ;
#4911 = CIRCLE('',#13950,0.15) ;
#4912 = CIRCLE('',#13953,0.15) ;
#4913 = CIRCLE('',#13954,0.15) ;
#4914 = CIRCLE('',#13957,0.15) ;
#4915 = CIRCLE('',#13958,0.15) ;
#4916 = CIRCLE('',#13961,0.15) ;
#4917 = CIRCLE('',#13962,0.15) ;
#4918 = CIRCLE('',#13965,0.15) ;
#4919 = CIRCLE('',#13966,0.15) ;
#4920 = CIRCLE('',#13969,0.15) ;
#4921 = CIRCLE('',#13970,0.15) ;
#4922 = CIRCLE('',#13973,0.4) ;
#4923 = CIRCLE('',#13974,0.4) ;
#4924 = CIRCLE('',#13976,0.4) ;
#4925 = CIRCLE('',#13977,0.4) ;
#4926 = CIRCLE('',#13979,0.4) ;
#4927 = CIRCLE('',#13980,0.4) ;
#4928 = CIRCLE('',#13982,0.4) ;
#4929 = CIRCLE('',#13983,0.4) ;
#4930 = CIRCLE('',#13985,0.4) ;
#4931 = CIRCLE('',#13986,0.4) ;
#4932 = CIRCLE('',#13988,0.4) ;
#4933 = CIRCLE('',#13989,0.4) ;
#4934 = CIRCLE('',#13991,0.4) ;
#4935 = CIRCLE('',#13992,0.4) ;
#4936 = CIRCLE('',#13994,0.4) ;
#4937 = CIRCLE('',#13995,0.4) ;
#4938 = CIRCLE('',#13997,0.4) ;
#4939 = CIRCLE('',#13998,0.4) ;
#4940 = CIRCLE('',#14000,0.4) ;
#4941 = CIRCLE('',#14001,0.4) ;
#4942 = CIRCLE('',#14003,0.4) ;
#4943 = CIRCLE('',#14004,0.4) ;
#4944 = CIRCLE('',#14006,0.4) ;
#4945 = CIRCLE('',#14007,0.4) ;
#4946 = CIRCLE('',#14009,0.4) ;
#4947 = CIRCLE('',#14010,0.4) ;
#4948 = CIRCLE('',#14012,0.4) ;
#4949 = CIRCLE('',#14013,0.4) ;
#4950 = CIRCLE('',#14015,0.4) ;
#4951 = CIRCLE('',#14016,0.4) ;
#4952 = CIRCLE('',#14018,0.4) ;
#4953 = CIRCLE('',#14019,0.4) ;
#4954 = CIRCLE('',#14021,0.4) ;
#4955 = CIRCLE('',#14022,0.4) ;
#4956 = CIRCLE('',#14024,0.4) ;
#4957 = CIRCLE('',#14025,0.4) ;
#4958 = CIRCLE('',#14027,0.4) ;
#4959 = CIRCLE('',#14028,0.4) ;
#4960 = CIRCLE('',#14030,0.4) ;
#4961 = CIRCLE('',#14031,0.4) ;
#4962 = CIRCLE('',#14033,0.4) ;
#4963 = CIRCLE('',#14034,0.4) ;
#4964 = CIRCLE('',#14036,0.4) ;
#4965 = CIRCLE('',#14037,0.4) ;
#4966 = CIRCLE('',#14039,0.4) ;
#4967 = CIRCLE('',#14040,0.4) ;
#4968 = CIRCLE('',#14042,0.4) ;
#4969 = CIRCLE('',#14043,0.4) ;
#4970 = CIRCLE('',#14045,0.215) ;
#4971 = CIRCLE('',#14046,0.215) ;
#4972 = CIRCLE('',#14048,0.215) ;
#4973 = CIRCLE('',#14049,0.215) ;
#4974 = CIRCLE('',#14051,0.215) ;
#4975 = CIRCLE('',#14052,0.215) ;
#4976 = CIRCLE('',#14054,0.51) ;
#4977 = CIRCLE('',#14055,0.51) ;
#4978 = CIRCLE('',#14057,10.) ;
#4979 = CIRCLE('',#14058,10.) ;
#4980 = CIRCLE('',#14063,1.45) ;
#4981 = CIRCLE('',#14064,1.05) ;
#4982 = CIRCLE('',#14066,1.45) ;
#4983 = CIRCLE('',#14067,1.05) ;
#4984 = CIRCLE('',#14071,1.75) ;
#4985 = CIRCLE('',#14072,0.75) ;
#4986 = CIRCLE('',#14074,1.75) ;
#4987 = CIRCLE('',#14076,0.75) ;
#4988 = CIRCLE('',#14080,1.45) ;
#4989 = CIRCLE('',#14081,1.05) ;
#4990 = CIRCLE('',#14083,1.45) ;
#4991 = CIRCLE('',#14084,1.05) ;
#4992 = CIRCLE('',#14088,1.75) ;
#4993 = CIRCLE('',#14089,0.75) ;
#4994 = CIRCLE('',#14091,1.75) ;
#4995 = CIRCLE('',#14093,0.75) ;
#4996 = CIRCLE('',#14097,0.75) ;
#4997 = CIRCLE('',#14098,0.75) ;
#4998 = CIRCLE('',#14100,1.1) ;
#4999 = CIRCLE('',#14101,1.1) ;
#5000 = CIRCLE('',#14108,0.95) ;
#5001 = CIRCLE('',#14109,0.705) ;
#5002 = CIRCLE('',#14111,0.705) ;
#5003 = CIRCLE('',#14113,0.95) ;
#5004 = CIRCLE('',#14120,1.4) ;
#5005 = CIRCLE('',#14121,0.75) ;
#5006 = CIRCLE('',#14123,0.75) ;
#5007 = CIRCLE('',#14128,2.5) ;
#5008 = CIRCLE('',#14129,2.5) ;
#5009 = CIRCLE('',#14131,2.5) ;
#5010 = CIRCLE('',#14132,2.5) ;
#5011 = CIRCLE('',#14134,2.5) ;
#5012 = CIRCLE('',#14135,2.5) ;
#5013 = CIRCLE('',#14136,2.5) ;
#5014 = CIRCLE('',#14137,2.5) ;
#5015 = CIRCLE('',#14138,2.5) ;
#5016 = CIRCLE('',#14139,2.5) ;
#5017 = CIRCLE('',#14140,2.5) ;
#5018 = CIRCLE('',#14141,2.5) ;
#5019 = CIRCLE('',#14142,2.5) ;
#5020 = CIRCLE('',#14143,2.5) ;
#5021 = CIRCLE('',#14148,2.5) ;
#5022 = CIRCLE('',#14153,2.5) ;
#5023 = CIRCLE('',#14158,2.5) ;
#5024 = CIRCLE('',#14163,2.5) ;
#5025 = CIRCLE('',#14168,2.5) ;
#5026 = CIRCLE('',#14173,2.5) ;
#5027 = CIRCLE('',#14178,2.5) ;
#5028 = CIRCLE('',#14183,2.5) ;
#5029 = CIRCLE('',#14188,2.5) ;
#5030 = CIRCLE('',#14193,2.5) ;
#5031 = CIRCLE('',#14198,1.4) ;
#5032 = CIRCLE('',#14209,10.2) ;
#5033 = CIRCLE('',#14210,10.2) ;
#5034 = CIRCLE('',#14212,11.1) ;
#5035 = CIRCLE('',#14213,11.1) ;
#5036 = CIRCLE('',#14229,0.25) ;
#5037 = CIRCLE('',#14230,0.25) ;
#5038 = CIRCLE('',#14233,0.21) ;
#5039 = CIRCLE('',#14234,0.21) ;
#5040 = CIRCLE('',#14236,0.5) ;
#5041 = CIRCLE('',#14237,0.5) ;
#5042 = CIRCLE('',#14239,0.5) ;
#5043 = CIRCLE('',#14240,0.5) ;
#5044 = CIRCLE('',#14242,0.5) ;
#5045 = CIRCLE('',#14243,0.5) ;
#5046 = CIRCLE('',#14255,0.2) ;
#5047 = CIRCLE('',#14256,0.2) ;
#5048 = CIRCLE('',#14261,0.05) ;
#5049 = CIRCLE('',#14262,0.05) ;
#5050 = CIRCLE('',#14264,0.05) ;
#5051 = CIRCLE('',#14265,0.05) ;
#5052 = CIRCLE('',#14266,0.05) ;
#5053 = CIRCLE('',#14267,0.0499999999999998) ;
#5054 = CIRCLE('',#14268,0.05) ;
#5055 = CIRCLE('',#14270,0.05) ;
#5056 = CIRCLE('',#14271,0.05) ;
#5057 = CIRCLE('',#14272,0.05) ;
#5058 = CIRCLE('',#14273,0.05) ;
#5059 = CIRCLE('',#14275,0.05) ;
#5060 = CIRCLE('',#14276,0.05) ;
#5061 = CIRCLE('',#14277,0.05) ;
#5062 = CIRCLE('',#14278,0.05) ;
#5063 = CIRCLE('',#14280,0.05) ;
#5064 = CIRCLE('',#14281,0.05) ;
#5065 = CIRCLE('',#14282,0.05) ;
#5066 = CIRCLE('',#14283,0.05) ;
#5067 = CIRCLE('',#14285,0.05) ;
#5068 = CIRCLE('',#14286,0.05) ;
#5069 = CIRCLE('',#14287,0.0499999999999998) ;
#5070 = CIRCLE('',#14288,0.05) ;
#5071 = CIRCLE('',#14289,0.05) ;
#5072 = CIRCLE('',#14291,0.05) ;
#5073 = CIRCLE('',#14292,0.05) ;
#5074 = CIRCLE('',#14294,0.05) ;
#5075 = CIRCLE('',#14295,0.05) ;
#5076 = CIRCLE('',#14297,0.05) ;
#5077 = CIRCLE('',#14298,0.05) ;
#5078 = CIRCLE('',#14300,0.05) ;
#5079 = CIRCLE('',#14301,0.05) ;
#5080 = CIRCLE('',#14302,0.05) ;
#5081 = CIRCLE('',#14303,0.0499999999999998) ;
#5082 = CIRCLE('',#14304,0.05) ;
#5083 = CIRCLE('',#14306,0.05) ;
#5084 = CIRCLE('',#14307,0.05) ;
#5085 = CIRCLE('',#14308,0.05) ;
#5086 = CIRCLE('',#14309,0.05) ;
#5087 = CIRCLE('',#14311,0.05) ;
#5088 = CIRCLE('',#14312,0.05) ;
#5089 = CIRCLE('',#14313,0.05) ;
#5090 = CIRCLE('',#14314,0.05) ;
#5091 = CIRCLE('',#14316,0.05) ;
#5092 = CIRCLE('',#14317,0.05) ;
#5093 = CIRCLE('',#14318,0.05) ;
#5094 = CIRCLE('',#14319,0.05) ;
#5095 = CIRCLE('',#14321,0.05) ;
#5096 = CIRCLE('',#14322,0.05) ;
#5097 = CIRCLE('',#14323,0.0499999999999998) ;
#5098 = CIRCLE('',#14324,0.05) ;
#5099 = CIRCLE('',#14325,0.05) ;
#5100 = CIRCLE('',#14327,0.05) ;
#5101 = CIRCLE('',#14328,0.05) ;
#5102 = CIRCLE('',#14330,0.05) ;
#5103 = CIRCLE('',#14331,0.05) ;
#5104 = CIRCLE('',#14333,0.05) ;
#5105 = CIRCLE('',#14334,0.05) ;
#5106 = CIRCLE('',#14336,0.05) ;
#5107 = CIRCLE('',#14337,0.05) ;
#5108 = CIRCLE('',#14338,0.05) ;
#5109 = CIRCLE('',#14339,0.0499999999999998) ;
#5110 = CIRCLE('',#14340,0.05) ;
#5111 = CIRCLE('',#14342,0.05) ;
#5112 = CIRCLE('',#14343,0.05) ;
#5113 = CIRCLE('',#14344,0.05) ;
#5114 = CIRCLE('',#14345,0.05) ;
#5115 = CIRCLE('',#14347,0.05) ;
#5116 = CIRCLE('',#14348,0.05) ;
#5117 = CIRCLE('',#14349,0.05) ;
#5118 = CIRCLE('',#14350,0.05) ;
#5119 = CIRCLE('',#14352,0.05) ;
#5120 = CIRCLE('',#14353,0.05) ;
#5121 = CIRCLE('',#14354,0.05) ;
#5122 = CIRCLE('',#14355,0.05) ;
#5123 = CIRCLE('',#14357,0.05) ;
#5124 = CIRCLE('',#14358,0.05) ;
#5125 = CIRCLE('',#14359,0.0499999999999998) ;
#5126 = CIRCLE('',#14360,0.05) ;
#5127 = CIRCLE('',#14361,0.05) ;
#5128 = CIRCLE('',#14363,0.05) ;
#5129 = CIRCLE('',#14364,0.05) ;
#5130 = CIRCLE('',#14366,0.05) ;
#5131 = CIRCLE('',#14367,0.05) ;
#5132 = CIRCLE('',#14369,0.05) ;
#5133 = CIRCLE('',#14370,0.05) ;
#5134 = CIRCLE('',#14372,0.05) ;
#5135 = CIRCLE('',#14373,0.05) ;
#5136 = CIRCLE('',#14374,0.05) ;
#5137 = CIRCLE('',#14375,0.0499999999999998) ;
#5138 = CIRCLE('',#14376,0.05) ;
#5139 = CIRCLE('',#14378,0.05) ;
#5140 = CIRCLE('',#14379,0.05) ;
#5141 = CIRCLE('',#14380,0.05) ;
#5142 = CIRCLE('',#14381,0.05) ;
#5143 = CIRCLE('',#14383,0.05) ;
#5144 = CIRCLE('',#14384,0.05) ;
#5145 = CIRCLE('',#14385,0.05) ;
#5146 = CIRCLE('',#14386,0.05) ;
#5147 = CIRCLE('',#14388,0.05) ;
#5148 = CIRCLE('',#14389,0.05) ;
#5149 = CIRCLE('',#14390,0.05) ;
#5150 = CIRCLE('',#14391,0.05) ;
#5151 = CIRCLE('',#14393,0.05) ;
#5152 = CIRCLE('',#14394,0.05) ;
#5153 = CIRCLE('',#14395,0.0499999999999998) ;
#5154 = CIRCLE('',#14396,0.05) ;
#5155 = CIRCLE('',#14397,0.05) ;
#5156 = CIRCLE('',#14399,0.05) ;
#5157 = CIRCLE('',#14400,0.05) ;
#5158 = CIRCLE('',#14402,0.05) ;
#5159 = CIRCLE('',#14493,0.05) ;
#5160 = CIRCLE('',#14497,1.00181590545205) ;
#5161 = CIRCLE('',#14498,1.1) ;
#5162 = CIRCLE('',#14500,1.4) ;
#5163 = CIRCLE('',#14502,0.834979872033575) ;
#5164 = CIRCLE('',#14503,1.1) ;
#5165 = CIRCLE('',#14505,1.1) ;
#5166 = CIRCLE('',#14507,1.00181590545205) ;
#5167 = CIRCLE('',#14509,1.1) ;
#5168 = CIRCLE('',#14512,1.00181590545205) ;
#5169 = CIRCLE('',#14513,1.4) ;
#5170 = CIRCLE('',#14515,1.1) ;
#5171 = CIRCLE('',#14516,1.00181590545205) ;
#5172 = CIRCLE('',#14518,1.4) ;
#5173 = CIRCLE('',#14521,1.00181590545205) ;
#5174 = CIRCLE('',#14522,1.1) ;
#5175 = CIRCLE('',#14523,1.00181590545205) ;
#5176 = CIRCLE('',#14525,1.4) ;
#5177 = CIRCLE('',#14527,1.4) ;
#5178 = CIRCLE('',#14529,0.834979872033575) ;
#5179 = CIRCLE('',#14530,1.1) ;
#5180 = CIRCLE('',#14532,1.1) ;
#5181 = CIRCLE('',#14534,1.00181590545205) ;
#5182 = CIRCLE('',#14535,1.4) ;
#5183 = CIRCLE('',#14537,1.1) ;
#5184 = CIRCLE('',#14538,1.00181590545205) ;
#5185 = CIRCLE('',#14540,1.4) ;
#5186 = CIRCLE('',#14542,1.00181590545205) ;
#5187 = CIRCLE('',#14543,1.1) ;
#5188 = CIRCLE('',#14544,1.00181590545205) ;
#5189 = CIRCLE('',#14546,1.4) ;
#5190 = CIRCLE('',#14548,1.4) ;
#5191 = CIRCLE('',#14550,0.834979872033577) ;
#5192 = CIRCLE('',#14551,1.1) ;
#5193 = CIRCLE('',#14553,1.1) ;
#5194 = CIRCLE('',#14555,1.00181590545205) ;
#5195 = CIRCLE('',#14556,1.4) ;
#5196 = CIRCLE('',#14558,1.1) ;
#5197 = CIRCLE('',#14559,1.00181590545205) ;
#5198 = CIRCLE('',#14561,1.4) ;
#5199 = CIRCLE('',#14563,1.00181590545205) ;
#5200 = CIRCLE('',#14564,1.1) ;
#5201 = CIRCLE('',#14565,1.00181590545205) ;
#5202 = CIRCLE('',#14567,1.4) ;
#5203 = CIRCLE('',#14569,1.4) ;
#5204 = CIRCLE('',#14571,0.834979872033573) ;
#5205 = CIRCLE('',#14572,1.1) ;
#5206 = CIRCLE('',#14574,1.1) ;
#5207 = CIRCLE('',#14576,1.00181590545205) ;
#5208 = CIRCLE('',#14577,1.4) ;
#5209 = CIRCLE('',#14579,1.1) ;
#5210 = CIRCLE('',#14580,1.00181590545205) ;
#5211 = CIRCLE('',#14582,1.4) ;
#5212 = CIRCLE('',#14584,1.00181590545205) ;
#5213 = CIRCLE('',#14585,1.1) ;
#5214 = CIRCLE('',#14586,1.00181590545205) ;
#5215 = CIRCLE('',#14588,1.4) ;
#5216 = CIRCLE('',#14591,0.834979872033577) ;
#5217 = CIRCLE('',#14594,1.00181590545205) ;
#5218 = CIRCLE('',#14596,1.1) ;
#5219 = CIRCLE('',#14597,1.00181590545205) ;
#5220 = CIRCLE('',#14600,1.00181590545205) ;
#5221 = CIRCLE('',#14601,1.1) ;
#5222 = CIRCLE('',#14602,1.00181590545205) ;
#5223 = CIRCLE('',#14606,0.834979872033575) ;
#5224 = CIRCLE('',#14609,1.00181590545205) ;
#5225 = CIRCLE('',#14611,1.00181590545205) ;
#5226 = CIRCLE('',#14612,1.1) ;
#5227 = CIRCLE('',#14613,1.00181590545205) ;
#5228 = CIRCLE('',#14614,1.1) ;
#5229 = CIRCLE('',#14617,1.00181590545205) ;
#5230 = CIRCLE('',#14618,1.1) ;
#5231 = CIRCLE('',#14619,1.00181590545205) ;
#5232 = CIRCLE('',#14620,1.1) ;
#5233 = CIRCLE('',#14621,1.00181590545205) ;
#5234 = CIRCLE('',#14625,0.834979872033575) ;
#5235 = CIRCLE('',#14628,1.00181590545205) ;
#5236 = CIRCLE('',#14629,1.1) ;
#5237 = CIRCLE('',#14633,0.834979872033575) ;
#5238 = CIRCLE('',#14636,1.00181590545205) ;
#5239 = CIRCLE('',#14637,1.00181590545205) ;
#5240 = CIRCLE('',#14639,1.1) ;
#5241 = CIRCLE('',#14640,1.1) ;
#5242 = CIRCLE('',#14642,1.00181590545205) ;
#5243 = CIRCLE('',#14643,1.4) ;
#5244 = CIRCLE('',#14645,1.00181590545205) ;
#5245 = CIRCLE('',#14646,1.1) ;
#5246 = CIRCLE('',#14647,1.00181590545205) ;
#5247 = CIRCLE('',#14648,1.1) ;
#5248 = CIRCLE('',#14652,1.4) ;
#5249 = CIRCLE('',#14653,1.4) ;
#5250 = CIRCLE('',#14654,1.4) ;
#5251 = CIRCLE('',#14655,1.4) ;
#5252 = CIRCLE('',#14657,1.4) ;
#5253 = CIRCLE('',#14658,1.4) ;
#5254 = CIRCLE('',#14659,1.4) ;
#5255 = CIRCLE('',#14660,1.4) ;
#5256 = CIRCLE('',#14662,1.4) ;
#5257 = CIRCLE('',#14663,1.4) ;
#5258 = CIRCLE('',#14664,1.4) ;
#5259 = CIRCLE('',#14665,1.4) ;
#5260 = CIRCLE('',#14667,1.4) ;
#5261 = CIRCLE('',#14668,1.4) ;
#5262 = CIRCLE('',#14669,1.4) ;
#5263 = CIRCLE('',#14670,1.4) ;
#5264 = CIRCLE('',#14672,1.4) ;
#5265 = CIRCLE('',#14673,1.4) ;
#5266 = CIRCLE('',#14674,1.4) ;
#5267 = CIRCLE('',#14675,1.4) ;
#5268 = CIRCLE('',#14677,1.4) ;
#5269 = CIRCLE('',#14678,1.4) ;
#5270 = CIRCLE('',#14679,1.4) ;
#5271 = CIRCLE('',#14680,1.4) ;
#5272 = CIRCLE('',#14682,1.4) ;
#5273 = CIRCLE('',#14683,1.1) ;
#5274 = CIRCLE('',#14685,1.4) ;
#5275 = CIRCLE('',#14686,1.4) ;
#5276 = CIRCLE('',#14687,1.4) ;
#5277 = CIRCLE('',#14688,1.4) ;
#5278 = CIRCLE('',#14690,1.1) ;
#5279 = CIRCLE('',#14692,1.4) ;
#5280 = CIRCLE('',#14694,1.4) ;
#5281 = CIRCLE('',#14695,1.4) ;
#5282 = CIRCLE('',#14698,1.1) ;
#5283 = CIRCLE('',#14701,1.4) ;
#5284 = CIRCLE('',#14703,1.4) ;
#5285 = CIRCLE('',#14705,1.4) ;
#5286 = CIRCLE('',#14707,1.4) ;
#5287 = CIRCLE('',#14709,1.4) ;
#5288 = CIRCLE('',#14713,1.4) ;
#5289 = CIRCLE('',#14715,1.4) ;
#5290 = CIRCLE('',#14717,1.4) ;
#5291 = CIRCLE('',#14718,1.4) ;
#5292 = CIRCLE('',#14720,1.4) ;
#5293 = CIRCLE('',#14721,1.4) ;
#5294 = CIRCLE('',#14723,1.4) ;
#5295 = CIRCLE('',#14725,1.4) ;
#5296 = CIRCLE('',#14729,1.4) ;
#5297 = CIRCLE('',#14731,1.4) ;
#5298 = CIRCLE('',#14733,1.4) ;
#5299 = CIRCLE('',#14734,1.4) ;
#5300 = CIRCLE('',#14736,1.4) ;
#5301 = CIRCLE('',#14737,1.4) ;
#5302 = CIRCLE('',#14739,1.4) ;
#5303 = CIRCLE('',#14741,1.4) ;
#5304 = CIRCLE('',#14745,1.4) ;
#5305 = CIRCLE('',#14747,1.4) ;
#5306 = CIRCLE('',#14749,1.4) ;
#5307 = CIRCLE('',#14750,1.4) ;
#5308 = CIRCLE('',#14752,1.4) ;
#5309 = CIRCLE('',#14753,1.4) ;
#5310 = CIRCLE('',#14755,1.4) ;
#5311 = CIRCLE('',#14758,1.4) ;
#5312 = CIRCLE('',#14761,1.4) ;
#5313 = CIRCLE('',#14770,1.4) ;
#5314 = CIRCLE('',#14772,1.1) ;
#5315 = CIRCLE('',#14774,1.4) ;
#5316 = CIRCLE('',#14777,0.834979872033575) ;
#5317 = CIRCLE('',#14780,0.834979872033575) ;
#5318 = CIRCLE('',#14783,0.834979872033573) ;
#5319 = CIRCLE('',#14784,1.1) ;
#5320 = CIRCLE('',#14786,1.1) ;
#5321 = CIRCLE('',#14788,0.834979872033575) ;
#5322 = CIRCLE('',#14789,1.1) ;
#5323 = CIRCLE('',#14791,1.1) ;
#5324 = CIRCLE('',#14793,0.834979872033573) ;
#5325 = CIRCLE('',#14794,1.1) ;
#5326 = CIRCLE('',#14796,1.1) ;
#5327 = CIRCLE('',#14798,0.834979872033575) ;
#5328 = CIRCLE('',#14799,1.1) ;
#5329 = CIRCLE('',#14801,1.1) ;
#5330 = CIRCLE('',#14804,0.45) ;
#5331 = CIRCLE('',#14805,0.45) ;
#5332 = CIRCLE('',#14808,0.45) ;
#5333 = CIRCLE('',#14809,0.45) ;
#5334 = CIRCLE('',#14812,0.425) ;
#5335 = CIRCLE('',#14813,0.425) ;
#5336 = CIRCLE('',#14815,0.45) ;
#5337 = CIRCLE('',#14816,0.45) ;
#5338 = CIRCLE('',#14819,0.45) ;
#5339 = CIRCLE('',#14820,0.45) ;
#5340 = CIRCLE('',#14823,0.425) ;
#5341 = CIRCLE('',#14824,0.425) ;
#5342 = CIRCLE('',#14858,1.75) ;
#5343 = CIRCLE('',#14859,1.75) ;
#5344 = CIRCLE('',#14860,1.75) ;
#5345 = CIRCLE('',#14861,1.75) ;
#5346 = CIRCLE('',#14865,0.7) ;
#5347 = CIRCLE('',#14866,0.7) ;
#5348 = CIRCLE('',#14888,1.6) ;
#5349 = CIRCLE('',#14890,1.6) ;
#5350 = CIRCLE('',#14892,1.6) ;
#5351 = CIRCLE('',#14894,1.8) ;
#5352 = CIRCLE('',#14896,1.8) ;
#5353 = CIRCLE('',#14898,1.8) ;
#5354 = CIRCLE('',#14900,1.8) ;
#5355 = CIRCLE('',#14903,1.6) ;
#5356 = CIRCLE('',#14906,1.8) ;
#5357 = CIRCLE('',#14908,1.8) ;
#5358 = CIRCLE('',#14910,1.8) ;
#5359 = CIRCLE('',#14911,1.8) ;
#5360 = CIRCLE('',#14913,1.8) ;
#5361 = CIRCLE('',#14915,1.8) ;
#5362 = CIRCLE('',#14917,1.3) ;
#5363 = CIRCLE('',#14919,0.6) ;
#5364 = CIRCLE('',#14920,0.6) ;
#5365 = CIRCLE('',#14922,0.6) ;
#5366 = CIRCLE('',#14923,0.6) ;
#5367 = CIRCLE('',#14925,1.6) ;
#5368 = CIRCLE('',#14926,1.6) ;
#5369 = CIRCLE('',#14930,1.8) ;
#5370 = CIRCLE('',#14932,1.8) ;
#5371 = CIRCLE('',#14941,0.4) ;
#5372 = CIRCLE('',#14942,0.4) ;
#5373 = CIRCLE('',#14944,0.3) ;
#5374 = CIRCLE('',#14945,0.3) ;
#5375 = CIRCLE('',#14947,1.5) ;
#5376 = CIRCLE('',#14948,0.3) ;
#5377 = CIRCLE('',#14949,1.5) ;
#5378 = CIRCLE('',#14950,0.3) ;
#5379 = CIRCLE('',#14951,1.5) ;
#5380 = CIRCLE('',#14952,0.3) ;
#5381 = CIRCLE('',#14953,1.5) ;
#5382 = CIRCLE('',#14954,0.3) ;
#5383 = CIRCLE('',#14955,1.5) ;
#5384 = CIRCLE('',#14956,0.3) ;
#5385 = CIRCLE('',#14957,1.5) ;
#5386 = CIRCLE('',#14958,0.3) ;
#5387 = CIRCLE('',#14959,1.5) ;
#5388 = CIRCLE('',#14960,0.3) ;
#5389 = CIRCLE('',#14961,1.5) ;
#5390 = CIRCLE('',#14963,1.5) ;
#5391 = CIRCLE('',#14965,0.3) ;
#5392 = CIRCLE('',#14967,1.5) ;
#5393 = CIRCLE('',#14969,0.3) ;
#5394 = CIRCLE('',#14971,1.5) ;
#5395 = CIRCLE('',#14973,0.3) ;
#5396 = CIRCLE('',#14975,1.5) ;
#5397 = CIRCLE('',#14977,0.3) ;
#5398 = CIRCLE('',#14979,1.5) ;
#5399 = CIRCLE('',#14981,0.3) ;
#5400 = CIRCLE('',#14983,1.5) ;
#5401 = CIRCLE('',#14985,0.3) ;
#5402 = CIRCLE('',#14987,1.5) ;
#5403 = CIRCLE('',#14989,0.3) ;
#5404 = CIRCLE('',#14991,1.5) ;
#5405 = CIRCLE('',#14995,0.4) ;
#5406 = CIRCLE('',#14996,0.4) ;
#5407 = CIRCLE('',#15001,0.4) ;
#5408 = CIRCLE('',#15002,0.4) ;
#5409 = CIRCLE('',#15004,0.6) ;
#5410 = CIRCLE('',#15005,0.6) ;
#5411 = CIRCLE('',#15010,0.4) ;
#5412 = CIRCLE('',#15011,0.4) ;
#5413 = CIRCLE('',#15013,0.8) ;
#5414 = CIRCLE('',#15014,0.8) ;
#5415 = CIRCLE('',#15017,1.5) ;
#5416 = CIRCLE('',#15021,1.5) ;
#5417 = CIRCLE('',#15024,1.5) ;
#5418 = CIRCLE('',#15028,1.5) ;
#5419 = CIRCLE('',#15031,1.5) ;
#5420 = CIRCLE('',#15035,1.5) ;
#5421 = CIRCLE('',#15038,1.5) ;
#5422 = CIRCLE('',#15042,1.5) ;
#5423 = CIRCLE('',#15045,1.5) ;
#5424 = CIRCLE('',#15046,1.5) ;
#5425 = CIRCLE('',#15050,1.5) ;
#5426 = CIRCLE('',#15051,1.5) ;
#5427 = CIRCLE('',#15054,1.5) ;
#5428 = CIRCLE('',#15058,1.5) ;
#5429 = CIRCLE('',#15061,1.5) ;
#5430 = CIRCLE('',#15065,1.5) ;
#5431 = CIRCLE('',#15068,1.5) ;
#5432 = CIRCLE('',#15072,1.5) ;
#5433 = CIRCLE('',#15075,1.5) ;
#5434 = CIRCLE('',#15079,1.5) ;
#5435 = CIRCLE('',#15082,1.5) ;
#5436 = CIRCLE('',#15086,1.5) ;
#5437 = CIRCLE('',#15089,1.5) ;
#5438 = CIRCLE('',#15090,1.5) ;
#5439 = CIRCLE('',#15095,1.) ;
#5440 = CIRCLE('',#15096,1.) ;
#5441 = CIRCLE('',#15098,1.29) ;
#5442 = CIRCLE('',#15099,1.29) ;
#5443 = CIRCLE('',#15104,1.4) ;
#5444 = CIRCLE('',#15105,1.23) ;
#5445 = CIRCLE('',#15107,1.4) ;
#5446 = CIRCLE('',#15110,1.23) ;
#5447 = CIRCLE('',#15113,1.4) ;
#5448 = CIRCLE('',#15115,1.4) ;
#5449 = CIRCLE('',#15118,1.4) ;
#5450 = CIRCLE('',#15120,1.31) ;
#5451 = CIRCLE('',#15122,1.4) ;
#5452 = CIRCLE('',#15124,1.4) ;
#5453 = CIRCLE('',#15125,1.4) ;
#5454 = CIRCLE('',#15126,1.4) ;
#5455 = CIRCLE('',#15127,1.4) ;
#5456 = CIRCLE('',#15128,1.4) ;
#5457 = CIRCLE('',#15130,1.4) ;
#5458 = CIRCLE('',#15131,1.4) ;
#5459 = CIRCLE('',#15139,1.31) ;
#5460 = CIRCLE('',#15141,1.4) ;
#5461 = CIRCLE('',#15149,1.75) ;
#5462 = CIRCLE('',#15150,1.41) ;
#5463 = CIRCLE('',#15152,1.41) ;
#5464 = CIRCLE('',#15154,1.75) ;
#5465 = CIRCLE('',#15162,1.75) ;
#5466 = CIRCLE('',#15163,1.75) ;
#5467 = CIRCLE('',#15165,1.41) ;
#5468 = CIRCLE('',#15166,1.41) ;
#5469 = CIRCLE('',#15185,1.45) ;
#5470 = CIRCLE('',#15186,1.45) ;
#5471 = CIRCLE('',#15188,1.75) ;
#5472 = CIRCLE('',#15189,1.75) ;
#5473 = CIRCLE('',#15194,1.1) ;
#5474 = CIRCLE('',#15195,1.1) ;
#5475 = CIRCLE('',#15197,1.1) ;
#5476 = CIRCLE('',#15199,1.1) ;
#5477 = CIRCLE('',#15202,0.7) ;
#5478 = CIRCLE('',#15203,0.7) ;
#5479 = CIRCLE('',#15205,1.45) ;
#5480 = CIRCLE('',#15206,1.) ;
#5481 = CIRCLE('',#15209,1.) ;
#5482 = CIRCLE('',#15211,1.45) ;
#5483 = CIRCLE('',#15215,0.85) ;
#5484 = CIRCLE('',#15216,0.85) ;
#5485 = CIRCLE('',#15218,1.09) ;
#5486 = CIRCLE('',#15219,1.09) ;
#5487 = CIRCLE('',#15224,0.35) ;
#5488 = CIRCLE('',#15225,0.35) ;
#5489 = CIRCLE('',#15227,0.35) ;
#5490 = CIRCLE('',#15228,0.35) ;
#5491 = CIRCLE('',#15230,0.35) ;
#5492 = CIRCLE('',#15231,0.35) ;
#5493 = CIRCLE('',#15233,0.35) ;
#5494 = CIRCLE('',#15234,0.35) ;
#5495 = CIRCLE('',#15236,1.75) ;
#5496 = CIRCLE('',#15237,1.75) ;
#5497 = CIRCLE('',#15239,3.5) ;
#5498 = CIRCLE('',#15240,3.5) ;
#5499 = CIRCLE('',#15245,0.35) ;
#5500 = CIRCLE('',#15246,0.35) ;
#5501 = CIRCLE('',#15248,0.35) ;
#5502 = CIRCLE('',#15249,0.35) ;
#5503 = CIRCLE('',#15251,0.35) ;
#5504 = CIRCLE('',#15252,0.35) ;
#5505 = CIRCLE('',#15254,0.35) ;
#5506 = CIRCLE('',#15255,0.35) ;
#5507 = CIRCLE('',#15257,1.75) ;
#5508 = CIRCLE('',#15258,1.75) ;
#5509 = CIRCLE('',#15260,3.5) ;
#5510 = CIRCLE('',#15261,3.5) ;
#5511 = CIRCLE('',#15266,0.325) ;
#5512 = CIRCLE('',#15268,0.325) ;
#5513 = CIRCLE('',#15269,0.325) ;
#5514 = CIRCLE('',#15272,0.325) ;
#5515 = CIRCLE('',#15274,0.325) ;
#5516 = CIRCLE('',#15275,0.325) ;
#5517 = CIRCLE('',#15283,2.05) ;
#5518 = CIRCLE('',#15284,1.75) ;
#5519 = CIRCLE('',#15286,2.05) ;
#5520 = CIRCLE('',#15288,1.75) ;
#5521 = CIRCLE('',#15300,0.195) ;
#5522 = CIRCLE('',#15301,0.195) ;
#5523 = CIRCLE('',#15304,0.35) ;
#5524 = CIRCLE('',#15305,0.35) ;
#5525 = CIRCLE('',#15310,0.525) ;
#5526 = CIRCLE('',#15311,0.525) ;
#5527 = CIRCLE('',#15313,1.) ;
#5528 = CIRCLE('',#15314,1.) ;
#5529 = CIRCLE('',#15319,0.5) ;
#5530 = CIRCLE('',#15320,0.5) ;
#5531 = CIRCLE('',#15331,0.4) ;
#5532 = CIRCLE('',#15332,0.4) ;
#5533 = CIRCLE('',#15344,0.3) ;
#5534 = CIRCLE('',#15345,0.3) ;
#5535 = CIRCLE('',#15357,0.3) ;
#5536 = CIRCLE('',#15358,0.3) ;
#5537 = VERTEX_POINT('',#19706) ;
#5538 = VERTEX_POINT('',#19707) ;
#5539 = VERTEX_POINT('',#19709) ;
#5540 = VERTEX_POINT('',#19713) ;
#5541 = VERTEX_POINT('',#19716) ;
#5542 = VERTEX_POINT('',#19718) ;
#5543 = VERTEX_POINT('',#19722) ;
#5544 = VERTEX_POINT('',#19724) ;
#5545 = VERTEX_POINT('',#19726) ;
#5546 = VERTEX_POINT('',#19728) ;
#5547 = VERTEX_POINT('',#19730) ;
#5548 = VERTEX_POINT('',#19732) ;
#5549 = VERTEX_POINT('',#19735) ;
#5550 = VERTEX_POINT('',#19737) ;
#5551 = VERTEX_POINT('',#19739) ;
#5552 = VERTEX_POINT('',#19741) ;
#5553 = VERTEX_POINT('',#19744) ;
#5554 = VERTEX_POINT('',#19745) ;
#5555 = VERTEX_POINT('',#19762) ;
#5556 = VERTEX_POINT('',#19779) ;
#5557 = VERTEX_POINT('',#19781) ;
#5558 = VERTEX_POINT('',#19807) ;
#5559 = VERTEX_POINT('',#19809) ;
#5560 = VERTEX_POINT('',#19816) ;
#5561 = VERTEX_POINT('',#19819) ;
#5562 = VERTEX_POINT('',#19822) ;
#5563 = VERTEX_POINT('',#19824) ;
#5564 = VERTEX_POINT('',#19828) ;
#5565 = VERTEX_POINT('',#19830) ;
#5566 = VERTEX_POINT('',#19834) ;
#5567 = VERTEX_POINT('',#19836) ;
#5568 = VERTEX_POINT('',#19840) ;
#5569 = VERTEX_POINT('',#19842) ;
#5570 = VERTEX_POINT('',#19846) ;
#5571 = VERTEX_POINT('',#19848) ;
#5572 = VERTEX_POINT('',#19852) ;
#5573 = VERTEX_POINT('',#19854) ;
#5574 = VERTEX_POINT('',#19858) ;
#5575 = VERTEX_POINT('',#19859) ;
#5576 = VERTEX_POINT('',#19861) ;
#5577 = VERTEX_POINT('',#19863) ;
#5578 = VERTEX_POINT('',#19865) ;
#5579 = VERTEX_POINT('',#19867) ;
#5580 = VERTEX_POINT('',#19871) ;
#5581 = VERTEX_POINT('',#19873) ;
#5582 = VERTEX_POINT('',#19877) ;
#5583 = VERTEX_POINT('',#19881) ;
#5584 = VERTEX_POINT('',#19882) ;
#5585 = VERTEX_POINT('',#19889) ;
#5586 = VERTEX_POINT('',#19893) ;
#5587 = VERTEX_POINT('',#19897) ;
#5588 = VERTEX_POINT('',#19899) ;
#5589 = VERTEX_POINT('',#19902) ;
#5590 = VERTEX_POINT('',#19904) ;
#5591 = VERTEX_POINT('',#19906) ;
#5592 = VERTEX_POINT('',#19908) ;
#5593 = VERTEX_POINT('',#19911) ;
#5594 = VERTEX_POINT('',#19912) ;
#5595 = VERTEX_POINT('',#19966) ;
#5596 = VERTEX_POINT('',#19971) ;
#5597 = VERTEX_POINT('',#19981) ;
#5598 = VERTEX_POINT('',#19987) ;
#5599 = VERTEX_POINT('',#19989) ;
#5600 = VERTEX_POINT('',#19995) ;
#5601 = VERTEX_POINT('',#19998) ;
#5602 = VERTEX_POINT('',#20000) ;
#5603 = VERTEX_POINT('',#20004) ;
#5604 = VERTEX_POINT('',#20006) ;
#5605 = VERTEX_POINT('',#20011) ;
#5606 = VERTEX_POINT('',#20013) ;
#5607 = VERTEX_POINT('',#20018) ;
#5608 = VERTEX_POINT('',#20023) ;
#5609 = VERTEX_POINT('',#20030) ;
#5610 = VERTEX_POINT('',#20032) ;
#5611 = VERTEX_POINT('',#20036) ;
#5612 = VERTEX_POINT('',#20038) ;
#5613 = VERTEX_POINT('',#20042) ;
#5614 = VERTEX_POINT('',#20044) ;
#5615 = VERTEX_POINT('',#20048) ;
#5616 = VERTEX_POINT('',#20050) ;
#5617 = VERTEX_POINT('',#20054) ;
#5618 = VERTEX_POINT('',#20056) ;
#5619 = VERTEX_POINT('',#20060) ;
#5620 = VERTEX_POINT('',#20062) ;
#5621 = VERTEX_POINT('',#20066) ;
#5622 = VERTEX_POINT('',#20068) ;
#5623 = VERTEX_POINT('',#20072) ;
#5624 = VERTEX_POINT('',#20074) ;
#5625 = VERTEX_POINT('',#20078) ;
#5626 = VERTEX_POINT('',#20080) ;
#5627 = VERTEX_POINT('',#20085) ;
#5628 = VERTEX_POINT('',#20087) ;
#5629 = VERTEX_POINT('',#20091) ;
#5630 = VERTEX_POINT('',#20093) ;
#5631 = VERTEX_POINT('',#20098) ;
#5632 = VERTEX_POINT('',#20100) ;
#5633 = VERTEX_POINT('',#20104) ;
#5634 = VERTEX_POINT('',#20107) ;
#5635 = VERTEX_POINT('',#20111) ;
#5636 = VERTEX_POINT('',#20113) ;
#5637 = VERTEX_POINT('',#20118) ;
#5638 = VERTEX_POINT('',#20120) ;
#5639 = VERTEX_POINT('',#20127) ;
#5640 = VERTEX_POINT('',#20129) ;
#5641 = VERTEX_POINT('',#20136) ;
#5642 = VERTEX_POINT('',#20138) ;
#5643 = VERTEX_POINT('',#20142) ;
#5644 = VERTEX_POINT('',#20144) ;
#5645 = VERTEX_POINT('',#20148) ;
#5646 = VERTEX_POINT('',#20150) ;
#5647 = VERTEX_POINT('',#20154) ;
#5648 = VERTEX_POINT('',#20156) ;
#5649 = VERTEX_POINT('',#20160) ;
#5650 = VERTEX_POINT('',#20162) ;
#5651 = VERTEX_POINT('',#20166) ;
#5652 = VERTEX_POINT('',#20168) ;
#5653 = VERTEX_POINT('',#20172) ;
#5654 = VERTEX_POINT('',#20174) ;
#5655 = VERTEX_POINT('',#20178) ;
#5656 = VERTEX_POINT('',#20180) ;
#5657 = VERTEX_POINT('',#20187) ;
#5658 = VERTEX_POINT('',#20188) ;
#5659 = VERTEX_POINT('',#20190) ;
#5660 = VERTEX_POINT('',#20192) ;
#5661 = VERTEX_POINT('',#20196) ;
#5662 = VERTEX_POINT('',#20198) ;
#5663 = VERTEX_POINT('',#20202) ;
#5664 = VERTEX_POINT('',#20203) ;
#5665 = VERTEX_POINT('',#20210) ;
#5666 = VERTEX_POINT('',#20212) ;
#5667 = VERTEX_POINT('',#20217) ;
#5668 = VERTEX_POINT('',#20219) ;
#5669 = VERTEX_POINT('',#20224) ;
#5670 = VERTEX_POINT('',#20227) ;
#5671 = VERTEX_POINT('',#20231) ;
#5672 = VERTEX_POINT('',#20233) ;
#5673 = VERTEX_POINT('',#20237) ;
#5674 = VERTEX_POINT('',#20239) ;
#5675 = VERTEX_POINT('',#20243) ;
#5676 = VERTEX_POINT('',#20245) ;
#5677 = VERTEX_POINT('',#20249) ;
#5678 = VERTEX_POINT('',#20252) ;
#5679 = VERTEX_POINT('',#20256) ;
#5680 = VERTEX_POINT('',#20258) ;
#5681 = VERTEX_POINT('',#20266) ;
#5682 = VERTEX_POINT('',#20268) ;
#5683 = VERTEX_POINT('',#20273) ;
#5684 = VERTEX_POINT('',#20275) ;
#5685 = VERTEX_POINT('',#20280) ;
#5686 = VERTEX_POINT('',#20282) ;
#5687 = VERTEX_POINT('',#20287) ;
#5688 = VERTEX_POINT('',#20289) ;
#5689 = VERTEX_POINT('',#20294) ;
#5690 = VERTEX_POINT('',#20296) ;
#5691 = VERTEX_POINT('',#20301) ;
#5692 = VERTEX_POINT('',#20303) ;
#5693 = VERTEX_POINT('',#20308) ;
#5694 = VERTEX_POINT('',#20310) ;
#5695 = VERTEX_POINT('',#20315) ;
#5696 = VERTEX_POINT('',#20317) ;
#5697 = VERTEX_POINT('',#20322) ;
#5698 = VERTEX_POINT('',#20324) ;
#5699 = VERTEX_POINT('',#20329) ;
#5700 = VERTEX_POINT('',#20331) ;
#5701 = VERTEX_POINT('',#20336) ;
#5702 = VERTEX_POINT('',#20338) ;
#5703 = VERTEX_POINT('',#20343) ;
#5704 = VERTEX_POINT('',#20345) ;
#5705 = VERTEX_POINT('',#20350) ;
#5706 = VERTEX_POINT('',#20352) ;
#5707 = VERTEX_POINT('',#20357) ;
#5708 = VERTEX_POINT('',#20359) ;
#5709 = VERTEX_POINT('',#20364) ;
#5710 = VERTEX_POINT('',#20366) ;
#5711 = VERTEX_POINT('',#20371) ;
#5712 = VERTEX_POINT('',#20373) ;
#5713 = VERTEX_POINT('',#20378) ;
#5714 = VERTEX_POINT('',#20380) ;
#5715 = VERTEX_POINT('',#20385) ;
#5716 = VERTEX_POINT('',#20387) ;
#5717 = VERTEX_POINT('',#20392) ;
#5718 = VERTEX_POINT('',#20394) ;
#5719 = VERTEX_POINT('',#20399) ;
#5720 = VERTEX_POINT('',#20401) ;
#5721 = VERTEX_POINT('',#20406) ;
#5722 = VERTEX_POINT('',#20408) ;
#5723 = VERTEX_POINT('',#20413) ;
#5724 = VERTEX_POINT('',#20415) ;
#5725 = VERTEX_POINT('',#20420) ;
#5726 = VERTEX_POINT('',#20422) ;
#5727 = VERTEX_POINT('',#20427) ;
#5728 = VERTEX_POINT('',#20429) ;
#5729 = VERTEX_POINT('',#20434) ;
#5730 = VERTEX_POINT('',#20436) ;
#5731 = VERTEX_POINT('',#20440) ;
#5732 = VERTEX_POINT('',#20442) ;
#5733 = VERTEX_POINT('',#20446) ;
#5734 = VERTEX_POINT('',#20448) ;
#5735 = VERTEX_POINT('',#20452) ;
#5736 = VERTEX_POINT('',#20454) ;
#5737 = VERTEX_POINT('',#20458) ;
#5738 = VERTEX_POINT('',#20460) ;
#5739 = VERTEX_POINT('',#20464) ;
#5740 = VERTEX_POINT('',#20466) ;
#5741 = VERTEX_POINT('',#20470) ;
#5742 = VERTEX_POINT('',#20472) ;
#5743 = VERTEX_POINT('',#20476) ;
#5744 = VERTEX_POINT('',#20478) ;
#5745 = VERTEX_POINT('',#20482) ;
#5746 = VERTEX_POINT('',#20484) ;
#5747 = VERTEX_POINT('',#20488) ;
#5748 = VERTEX_POINT('',#20490) ;
#5749 = VERTEX_POINT('',#20494) ;
#5750 = VERTEX_POINT('',#20496) ;
#5751 = VERTEX_POINT('',#20500) ;
#5752 = VERTEX_POINT('',#20502) ;
#5753 = VERTEX_POINT('',#20506) ;
#5754 = VERTEX_POINT('',#20508) ;
#5755 = VERTEX_POINT('',#20512) ;
#5756 = VERTEX_POINT('',#20514) ;
#5757 = VERTEX_POINT('',#20518) ;
#5758 = VERTEX_POINT('',#20520) ;
#5759 = VERTEX_POINT('',#20524) ;
#5760 = VERTEX_POINT('',#20526) ;
#5761 = VERTEX_POINT('',#20530) ;
#5762 = VERTEX_POINT('',#20532) ;
#5763 = VERTEX_POINT('',#20536) ;
#5764 = VERTEX_POINT('',#20538) ;
#5765 = VERTEX_POINT('',#20542) ;
#5766 = VERTEX_POINT('',#20544) ;
#5767 = VERTEX_POINT('',#20548) ;
#5768 = VERTEX_POINT('',#20550) ;
#5769 = VERTEX_POINT('',#20554) ;
#5770 = VERTEX_POINT('',#20556) ;
#5771 = VERTEX_POINT('',#20560) ;
#5772 = VERTEX_POINT('',#20562) ;
#5773 = VERTEX_POINT('',#20566) ;
#5774 = VERTEX_POINT('',#20568) ;
#5775 = VERTEX_POINT('',#20572) ;
#5776 = VERTEX_POINT('',#20574) ;
#5777 = VERTEX_POINT('',#20578) ;
#5778 = VERTEX_POINT('',#20580) ;
#5779 = VERTEX_POINT('',#20584) ;
#5780 = VERTEX_POINT('',#20586) ;
#5781 = VERTEX_POINT('',#20590) ;
#5782 = VERTEX_POINT('',#20592) ;
#5783 = VERTEX_POINT('',#20596) ;
#5784 = VERTEX_POINT('',#20598) ;
#5785 = VERTEX_POINT('',#20602) ;
#5786 = VERTEX_POINT('',#20604) ;
#5787 = VERTEX_POINT('',#20611) ;
#5788 = VERTEX_POINT('',#20613) ;
#5789 = VERTEX_POINT('',#20616) ;
#5790 = VERTEX_POINT('',#20618) ;
#5791 = VERTEX_POINT('',#20625) ;
#5792 = VERTEX_POINT('',#20627) ;
#5793 = VERTEX_POINT('',#20630) ;
#5794 = VERTEX_POINT('',#20634) ;
#5795 = VERTEX_POINT('',#20640) ;
#5796 = VERTEX_POINT('',#20642) ;
#5797 = VERTEX_POINT('',#20645) ;
#5798 = VERTEX_POINT('',#20647) ;
#5799 = VERTEX_POINT('',#20654) ;
#5800 = VERTEX_POINT('',#20656) ;
#5801 = VERTEX_POINT('',#20659) ;
#5802 = VERTEX_POINT('',#20663) ;
#5803 = VERTEX_POINT('',#20669) ;
#5804 = VERTEX_POINT('',#20671) ;
#5805 = VERTEX_POINT('',#20675) ;
#5806 = VERTEX_POINT('',#20677) ;
#5807 = VERTEX_POINT('',#20684) ;
#5808 = VERTEX_POINT('',#20685) ;
#5809 = VERTEX_POINT('',#20687) ;
#5810 = VERTEX_POINT('',#20689) ;
#5811 = VERTEX_POINT('',#20693) ;
#5812 = VERTEX_POINT('',#20694) ;
#5813 = VERTEX_POINT('',#20696) ;
#5814 = VERTEX_POINT('',#20698) ;
#5815 = VERTEX_POINT('',#20711) ;
#5816 = VERTEX_POINT('',#20712) ;
#5817 = VERTEX_POINT('',#20714) ;
#5818 = VERTEX_POINT('',#20716) ;
#5819 = VERTEX_POINT('',#20720) ;
#5820 = VERTEX_POINT('',#20721) ;
#5821 = VERTEX_POINT('',#20723) ;
#5822 = VERTEX_POINT('',#20725) ;
#5823 = VERTEX_POINT('',#20732) ;
#5824 = VERTEX_POINT('',#20738) ;
#5825 = VERTEX_POINT('',#20739) ;
#5826 = VERTEX_POINT('',#20741) ;
#5827 = VERTEX_POINT('',#20743) ;
#5828 = VERTEX_POINT('',#20747) ;
#5829 = VERTEX_POINT('',#20748) ;
#5830 = VERTEX_POINT('',#20750) ;
#5831 = VERTEX_POINT('',#20752) ;
#5832 = VERTEX_POINT('',#20759) ;
#5833 = VERTEX_POINT('',#20761) ;
#5834 = VERTEX_POINT('',#20765) ;
#5835 = VERTEX_POINT('',#20767) ;
#5836 = VERTEX_POINT('',#20771) ;
#5837 = VERTEX_POINT('',#20773) ;
#5838 = VERTEX_POINT('',#20775) ;
#5839 = VERTEX_POINT('',#20777) ;
#5840 = VERTEX_POINT('',#20779) ;
#5841 = VERTEX_POINT('',#20781) ;
#5842 = VERTEX_POINT('',#20783) ;
#5843 = VERTEX_POINT('',#20785) ;
#5844 = VERTEX_POINT('',#20787) ;
#5845 = VERTEX_POINT('',#20789) ;
#5846 = VERTEX_POINT('',#20791) ;
#5847 = VERTEX_POINT('',#20793) ;
#5848 = VERTEX_POINT('',#20795) ;
#5849 = VERTEX_POINT('',#20797) ;
#5850 = VERTEX_POINT('',#20799) ;
#5851 = VERTEX_POINT('',#20801) ;
#5852 = VERTEX_POINT('',#20803) ;
#5853 = VERTEX_POINT('',#20805) ;
#5854 = VERTEX_POINT('',#20807) ;
#5855 = VERTEX_POINT('',#20809) ;
#5856 = VERTEX_POINT('',#20811) ;
#5857 = VERTEX_POINT('',#20813) ;
#5858 = VERTEX_POINT('',#20815) ;
#5859 = VERTEX_POINT('',#20817) ;
#5860 = VERTEX_POINT('',#20819) ;
#5861 = VERTEX_POINT('',#20821) ;
#5862 = VERTEX_POINT('',#20823) ;
#5863 = VERTEX_POINT('',#20825) ;
#5864 = VERTEX_POINT('',#20827) ;
#5865 = VERTEX_POINT('',#20829) ;
#5866 = VERTEX_POINT('',#20831) ;
#5867 = VERTEX_POINT('',#20833) ;
#5868 = VERTEX_POINT('',#20835) ;
#5869 = VERTEX_POINT('',#20837) ;
#5870 = VERTEX_POINT('',#20839) ;
#5871 = VERTEX_POINT('',#20841) ;
#5872 = VERTEX_POINT('',#20843) ;
#5873 = VERTEX_POINT('',#20845) ;
#5874 = VERTEX_POINT('',#20847) ;
#5875 = VERTEX_POINT('',#20849) ;
#5876 = VERTEX_POINT('',#20851) ;
#5877 = VERTEX_POINT('',#20853) ;
#5878 = VERTEX_POINT('',#20857) ;
#5879 = VERTEX_POINT('',#20861) ;
#5880 = VERTEX_POINT('',#20863) ;
#5881 = VERTEX_POINT('',#20869) ;
#5882 = VERTEX_POINT('',#20873) ;
#5883 = VERTEX_POINT('',#20875) ;
#5884 = VERTEX_POINT('',#20879) ;
#5885 = VERTEX_POINT('',#20885) ;
#5886 = VERTEX_POINT('',#20889) ;
#5887 = VERTEX_POINT('',#20893) ;
#5888 = VERTEX_POINT('',#20895) ;
#5889 = VERTEX_POINT('',#20901) ;
#5890 = VERTEX_POINT('',#20905) ;
#5891 = VERTEX_POINT('',#20907) ;
#5892 = VERTEX_POINT('',#20911) ;
#5893 = VERTEX_POINT('',#20917) ;
#5894 = VERTEX_POINT('',#20921) ;
#5895 = VERTEX_POINT('',#20925) ;
#5896 = VERTEX_POINT('',#20927) ;
#5897 = VERTEX_POINT('',#20933) ;
#5898 = VERTEX_POINT('',#20937) ;
#5899 = VERTEX_POINT('',#20939) ;
#5900 = VERTEX_POINT('',#20943) ;
#5901 = VERTEX_POINT('',#20949) ;
#5902 = VERTEX_POINT('',#20953) ;
#5903 = VERTEX_POINT('',#20957) ;
#5904 = VERTEX_POINT('',#20959) ;
#5905 = VERTEX_POINT('',#20965) ;
#5906 = VERTEX_POINT('',#20969) ;
#5907 = VERTEX_POINT('',#20971) ;
#5908 = VERTEX_POINT('',#20975) ;
#5909 = VERTEX_POINT('',#20981) ;
#5910 = VERTEX_POINT('',#20985) ;
#5911 = VERTEX_POINT('',#20989) ;
#5912 = VERTEX_POINT('',#20991) ;
#5913 = VERTEX_POINT('',#20997) ;
#5914 = VERTEX_POINT('',#21001) ;
#5915 = VERTEX_POINT('',#21003) ;
#5916 = VERTEX_POINT('',#21007) ;
#5917 = VERTEX_POINT('',#21013) ;
#5918 = VERTEX_POINT('',#21017) ;
#5919 = VERTEX_POINT('',#21021) ;
#5920 = VERTEX_POINT('',#21027) ;
#5921 = VERTEX_POINT('',#21033) ;
#5922 = VERTEX_POINT('',#21034) ;
#5923 = VERTEX_POINT('',#21036) ;
#5924 = VERTEX_POINT('',#21038) ;
#5925 = VERTEX_POINT('',#21042) ;
#5926 = VERTEX_POINT('',#21043) ;
#5927 = VERTEX_POINT('',#21045) ;
#5928 = VERTEX_POINT('',#21047) ;
#5929 = VERTEX_POINT('',#21060) ;
#5930 = VERTEX_POINT('',#21062) ;
#5931 = VERTEX_POINT('',#21066) ;
#5932 = VERTEX_POINT('',#21068) ;
#5933 = VERTEX_POINT('',#21075) ;
#5934 = VERTEX_POINT('',#21076) ;
#5935 = VERTEX_POINT('',#21078) ;
#5936 = VERTEX_POINT('',#21080) ;
#5937 = VERTEX_POINT('',#21084) ;
#5938 = VERTEX_POINT('',#21086) ;
#5939 = VERTEX_POINT('',#21090) ;
#5940 = VERTEX_POINT('',#21094) ;
#5941 = VERTEX_POINT('',#21098) ;
#5942 = VERTEX_POINT('',#21100) ;
#5943 = VERTEX_POINT('',#21102) ;
#5944 = VERTEX_POINT('',#21104) ;
#5945 = VERTEX_POINT('',#21108) ;
#5946 = VERTEX_POINT('',#21110) ;
#5947 = VERTEX_POINT('',#21114) ;
#5948 = VERTEX_POINT('',#21116) ;
#5949 = VERTEX_POINT('',#21126) ;
#5950 = VERTEX_POINT('',#21128) ;
#5951 = VERTEX_POINT('',#21133) ;
#5952 = VERTEX_POINT('',#21135) ;
#5953 = VERTEX_POINT('',#21139) ;
#5954 = VERTEX_POINT('',#21140) ;
#5955 = VERTEX_POINT('',#21142) ;
#5956 = VERTEX_POINT('',#21144) ;
#5957 = VERTEX_POINT('',#21148) ;
#5958 = VERTEX_POINT('',#21149) ;
#5959 = VERTEX_POINT('',#21151) ;
#5960 = VERTEX_POINT('',#21153) ;
#5961 = VERTEX_POINT('',#21157) ;
#5962 = VERTEX_POINT('',#21158) ;
#5963 = VERTEX_POINT('',#21160) ;
#5964 = VERTEX_POINT('',#21162) ;
#5965 = VERTEX_POINT('',#21166) ;
#5966 = VERTEX_POINT('',#21168) ;
#5967 = VERTEX_POINT('',#21172) ;
#5968 = VERTEX_POINT('',#21174) ;
#5969 = VERTEX_POINT('',#21178) ;
#5970 = VERTEX_POINT('',#21180) ;
#5971 = VERTEX_POINT('',#21185) ;
#5972 = VERTEX_POINT('',#21192) ;
#5973 = VERTEX_POINT('',#21202) ;
#5974 = VERTEX_POINT('',#21204) ;
#5975 = VERTEX_POINT('',#21211) ;
#5976 = VERTEX_POINT('',#21212) ;
#5977 = VERTEX_POINT('',#21216) ;
#5978 = VERTEX_POINT('',#21217) ;
#5979 = VERTEX_POINT('',#21219) ;
#5980 = VERTEX_POINT('',#21221) ;
#5981 = VERTEX_POINT('',#21223) ;
#5982 = VERTEX_POINT('',#21227) ;
#5983 = VERTEX_POINT('',#21228) ;
#5984 = VERTEX_POINT('',#21230) ;
#5985 = VERTEX_POINT('',#21232) ;
#5986 = VERTEX_POINT('',#21236) ;
#5987 = VERTEX_POINT('',#21237) ;
#5988 = VERTEX_POINT('',#21239) ;
#5989 = VERTEX_POINT('',#21241) ;
#5990 = VERTEX_POINT('',#21245) ;
#5991 = VERTEX_POINT('',#21246) ;
#5992 = VERTEX_POINT('',#21248) ;
#5993 = VERTEX_POINT('',#21250) ;
#5994 = VERTEX_POINT('',#21254) ;
#5995 = VERTEX_POINT('',#21255) ;
#5996 = VERTEX_POINT('',#21257) ;
#5997 = VERTEX_POINT('',#21259) ;
#5998 = VERTEX_POINT('',#21261) ;
#5999 = VERTEX_POINT('',#21265) ;
#6000 = VERTEX_POINT('',#21266) ;
#6001 = VERTEX_POINT('',#21270) ;
#6002 = VERTEX_POINT('',#21271) ;
#6003 = VERTEX_POINT('',#21275) ;
#6004 = VERTEX_POINT('',#21276) ;
#6005 = VERTEX_POINT('',#21280) ;
#6006 = VERTEX_POINT('',#21281) ;
#6007 = VERTEX_POINT('',#21283) ;
#6008 = VERTEX_POINT('',#21285) ;
#6009 = VERTEX_POINT('',#21287) ;
#6010 = VERTEX_POINT('',#21291) ;
#6011 = VERTEX_POINT('',#21292) ;
#6012 = VERTEX_POINT('',#21294) ;
#6013 = VERTEX_POINT('',#21296) ;
#6014 = VERTEX_POINT('',#21300) ;
#6015 = VERTEX_POINT('',#21301) ;
#6016 = VERTEX_POINT('',#21303) ;
#6017 = VERTEX_POINT('',#21305) ;
#6018 = VERTEX_POINT('',#21309) ;
#6019 = VERTEX_POINT('',#21310) ;
#6020 = VERTEX_POINT('',#21312) ;
#6021 = VERTEX_POINT('',#21314) ;
#6022 = VERTEX_POINT('',#21318) ;
#6023 = VERTEX_POINT('',#21319) ;
#6024 = VERTEX_POINT('',#21321) ;
#6025 = VERTEX_POINT('',#21323) ;
#6026 = VERTEX_POINT('',#21325) ;
#6027 = VERTEX_POINT('',#21329) ;
#6028 = VERTEX_POINT('',#21330) ;
#6029 = VERTEX_POINT('',#21334) ;
#6030 = VERTEX_POINT('',#21335) ;
#6031 = VERTEX_POINT('',#21339) ;
#6032 = VERTEX_POINT('',#21340) ;
#6033 = VERTEX_POINT('',#21344) ;
#6034 = VERTEX_POINT('',#21345) ;
#6035 = VERTEX_POINT('',#21347) ;
#6036 = VERTEX_POINT('',#21349) ;
#6037 = VERTEX_POINT('',#21351) ;
#6038 = VERTEX_POINT('',#21355) ;
#6039 = VERTEX_POINT('',#21356) ;
#6040 = VERTEX_POINT('',#21358) ;
#6041 = VERTEX_POINT('',#21360) ;
#6042 = VERTEX_POINT('',#21364) ;
#6043 = VERTEX_POINT('',#21365) ;
#6044 = VERTEX_POINT('',#21367) ;
#6045 = VERTEX_POINT('',#21369) ;
#6046 = VERTEX_POINT('',#21373) ;
#6047 = VERTEX_POINT('',#21374) ;
#6048 = VERTEX_POINT('',#21376) ;
#6049 = VERTEX_POINT('',#21378) ;
#6050 = VERTEX_POINT('',#21382) ;
#6051 = VERTEX_POINT('',#21383) ;
#6052 = VERTEX_POINT('',#21385) ;
#6053 = VERTEX_POINT('',#21387) ;
#6054 = VERTEX_POINT('',#21389) ;
#6055 = VERTEX_POINT('',#21393) ;
#6056 = VERTEX_POINT('',#21394) ;
#6057 = VERTEX_POINT('',#21398) ;
#6058 = VERTEX_POINT('',#21399) ;
#6059 = VERTEX_POINT('',#21403) ;
#6060 = VERTEX_POINT('',#21404) ;
#6061 = VERTEX_POINT('',#21408) ;
#6062 = VERTEX_POINT('',#21409) ;
#6063 = VERTEX_POINT('',#21411) ;
#6064 = VERTEX_POINT('',#21413) ;
#6065 = VERTEX_POINT('',#21415) ;
#6066 = VERTEX_POINT('',#21419) ;
#6067 = VERTEX_POINT('',#21420) ;
#6068 = VERTEX_POINT('',#21422) ;
#6069 = VERTEX_POINT('',#21424) ;
#6070 = VERTEX_POINT('',#21428) ;
#6071 = VERTEX_POINT('',#21429) ;
#6072 = VERTEX_POINT('',#21431) ;
#6073 = VERTEX_POINT('',#21433) ;
#6074 = VERTEX_POINT('',#21437) ;
#6075 = VERTEX_POINT('',#21438) ;
#6076 = VERTEX_POINT('',#21440) ;
#6077 = VERTEX_POINT('',#21442) ;
#6078 = VERTEX_POINT('',#21446) ;
#6079 = VERTEX_POINT('',#21447) ;
#6080 = VERTEX_POINT('',#21449) ;
#6081 = VERTEX_POINT('',#21451) ;
#6082 = VERTEX_POINT('',#21453) ;
#6083 = VERTEX_POINT('',#21457) ;
#6084 = VERTEX_POINT('',#21458) ;
#6085 = VERTEX_POINT('',#21462) ;
#6086 = VERTEX_POINT('',#21464) ;
#6087 = VERTEX_POINT('',#21466) ;
#6088 = VERTEX_POINT('',#21472) ;
#6089 = VERTEX_POINT('',#21487) ;
#6090 = VERTEX_POINT('',#21491) ;
#6091 = VERTEX_POINT('',#21493) ;
#6092 = VERTEX_POINT('',#21498) ;
#6093 = VERTEX_POINT('',#21503) ;
#6094 = VERTEX_POINT('',#21505) ;
#6095 = VERTEX_POINT('',#21510) ;
#6096 = VERTEX_POINT('',#21525) ;
#6097 = VERTEX_POINT('',#21529) ;
#6098 = VERTEX_POINT('',#21531) ;
#6099 = VERTEX_POINT('',#21536) ;
#6100 = VERTEX_POINT('',#21541) ;
#6101 = VERTEX_POINT('',#21543) ;
#6102 = VERTEX_POINT('',#21548) ;
#6103 = VERTEX_POINT('',#21563) ;
#6104 = VERTEX_POINT('',#21567) ;
#6105 = VERTEX_POINT('',#21569) ;
#6106 = VERTEX_POINT('',#21574) ;
#6107 = VERTEX_POINT('',#21579) ;
#6108 = VERTEX_POINT('',#21581) ;
#6109 = VERTEX_POINT('',#21586) ;
#6110 = VERTEX_POINT('',#21601) ;
#6111 = VERTEX_POINT('',#21605) ;
#6112 = VERTEX_POINT('',#21607) ;
#6113 = VERTEX_POINT('',#21612) ;
#6114 = VERTEX_POINT('',#21618) ;
#6115 = VERTEX_POINT('',#21620) ;
#6116 = VERTEX_POINT('',#21623) ;
#6117 = VERTEX_POINT('',#21626) ;
#6118 = VERTEX_POINT('',#21628) ;
#6119 = VERTEX_POINT('',#21631) ;
#6120 = VERTEX_POINT('',#21634) ;
#6121 = VERTEX_POINT('',#21635) ;
#6122 = VERTEX_POINT('',#21655) ;
#6123 = VERTEX_POINT('',#21657) ;
#6124 = VERTEX_POINT('',#21660) ;
#6125 = VERTEX_POINT('',#21662) ;
#6126 = VERTEX_POINT('',#21694) ;
#6127 = VERTEX_POINT('',#21696) ;
#6128 = VERTEX_POINT('',#21700) ;
#6129 = VERTEX_POINT('',#21703) ;
#6130 = VERTEX_POINT('',#21706) ;
#6131 = VERTEX_POINT('',#21708) ;
#6132 = VERTEX_POINT('',#21711) ;
#6133 = VERTEX_POINT('',#21714) ;
#6134 = VERTEX_POINT('',#21716) ;
#6135 = VERTEX_POINT('',#21719) ;
#6136 = VERTEX_POINT('',#21723) ;
#6137 = VERTEX_POINT('',#21726) ;
#6138 = VERTEX_POINT('',#21728) ;
#6139 = VERTEX_POINT('',#21732) ;
#6140 = VERTEX_POINT('',#21735) ;
#6141 = VERTEX_POINT('',#21738) ;
#6142 = VERTEX_POINT('',#21740) ;
#6143 = VERTEX_POINT('',#21743) ;
#6144 = VERTEX_POINT('',#21746) ;
#6145 = VERTEX_POINT('',#21748) ;
#6146 = VERTEX_POINT('',#21751) ;
#6147 = VERTEX_POINT('',#21755) ;
#6148 = VERTEX_POINT('',#21758) ;
#6149 = VERTEX_POINT('',#21760) ;
#6150 = VERTEX_POINT('',#21764) ;
#6151 = VERTEX_POINT('',#21767) ;
#6152 = VERTEX_POINT('',#21770) ;
#6153 = VERTEX_POINT('',#21772) ;
#6154 = VERTEX_POINT('',#21775) ;
#6155 = VERTEX_POINT('',#21778) ;
#6156 = VERTEX_POINT('',#21780) ;
#6157 = VERTEX_POINT('',#21783) ;
#6158 = VERTEX_POINT('',#21787) ;
#6159 = VERTEX_POINT('',#21790) ;
#6160 = VERTEX_POINT('',#21792) ;
#6161 = VERTEX_POINT('',#21796) ;
#6162 = VERTEX_POINT('',#21800) ;
#6163 = VERTEX_POINT('',#21804) ;
#6164 = VERTEX_POINT('',#21807) ;
#6165 = VERTEX_POINT('',#21812) ;
#6166 = VERTEX_POINT('',#21814) ;
#6167 = VERTEX_POINT('',#21816) ;
#6168 = VERTEX_POINT('',#21821) ;
#6169 = VERTEX_POINT('',#21825) ;
#6170 = VERTEX_POINT('',#21828) ;
#6171 = VERTEX_POINT('',#21829) ;
#6172 = VERTEX_POINT('',#21831) ;
#6173 = VERTEX_POINT('',#21834) ;
#6174 = VERTEX_POINT('',#21838) ;
#6175 = VERTEX_POINT('',#21839) ;
#6176 = VERTEX_POINT('',#21841) ;
#6177 = VERTEX_POINT('',#21844) ;
#6178 = VERTEX_POINT('',#21846) ;
#6179 = VERTEX_POINT('',#21851) ;
#6180 = VERTEX_POINT('',#21855) ;
#6181 = VERTEX_POINT('',#21856) ;
#6182 = VERTEX_POINT('',#21872) ;
#6183 = VERTEX_POINT('',#21876) ;
#6184 = VERTEX_POINT('',#21877) ;
#6185 = VERTEX_POINT('',#21881) ;
#6186 = VERTEX_POINT('',#21883) ;
#6187 = VERTEX_POINT('',#21886) ;
#6188 = VERTEX_POINT('',#21887) ;
#6189 = VERTEX_POINT('',#21891) ;
#6190 = VERTEX_POINT('',#21892) ;
#6191 = VERTEX_POINT('',#21894) ;
#6192 = VERTEX_POINT('',#21897) ;
#6193 = VERTEX_POINT('',#21924) ;
#6194 = VERTEX_POINT('',#21925) ;
#6195 = VERTEX_POINT('',#21927) ;
#6196 = VERTEX_POINT('',#21929) ;
#6197 = VERTEX_POINT('',#21933) ;
#6198 = VERTEX_POINT('',#21934) ;
#6199 = VERTEX_POINT('',#21936) ;
#6200 = VERTEX_POINT('',#21938) ;
#6201 = VERTEX_POINT('',#21942) ;
#6202 = VERTEX_POINT('',#21943) ;
#6203 = VERTEX_POINT('',#21945) ;
#6204 = VERTEX_POINT('',#21947) ;
#6205 = VERTEX_POINT('',#21951) ;
#6206 = VERTEX_POINT('',#21952) ;
#6207 = VERTEX_POINT('',#21954) ;
#6208 = VERTEX_POINT('',#21956) ;
#6209 = VERTEX_POINT('',#21960) ;
#6210 = VERTEX_POINT('',#21961) ;
#6211 = VERTEX_POINT('',#21963) ;
#6212 = VERTEX_POINT('',#21965) ;
#6213 = VERTEX_POINT('',#21969) ;
#6214 = VERTEX_POINT('',#21970) ;
#6215 = VERTEX_POINT('',#21972) ;
#6216 = VERTEX_POINT('',#21974) ;
#6217 = VERTEX_POINT('',#21978) ;
#6218 = VERTEX_POINT('',#21979) ;
#6219 = VERTEX_POINT('',#21983) ;
#6220 = VERTEX_POINT('',#21984) ;
#6221 = VERTEX_POINT('',#21986) ;
#6222 = VERTEX_POINT('',#21988) ;
#6223 = VERTEX_POINT('',#21992) ;
#6224 = VERTEX_POINT('',#21994) ;
#6225 = VERTEX_POINT('',#22027) ;
#6226 = VERTEX_POINT('',#22029) ;
#6227 = VERTEX_POINT('',#22031) ;
#6228 = VERTEX_POINT('',#22033) ;
#6229 = VERTEX_POINT('',#22035) ;
#6230 = VERTEX_POINT('',#22039) ;
#6231 = VERTEX_POINT('',#22042) ;
#6232 = VERTEX_POINT('',#22044) ;
#6233 = VERTEX_POINT('',#22046) ;
#6234 = VERTEX_POINT('',#22051) ;
#6235 = VERTEX_POINT('',#22052) ;
#6236 = VERTEX_POINT('',#22067) ;
#6237 = VERTEX_POINT('',#22086) ;
#6238 = VERTEX_POINT('',#22095) ;
#6239 = VERTEX_POINT('',#22097) ;
#6240 = VERTEX_POINT('',#22099) ;
#6241 = VERTEX_POINT('',#22103) ;
#6242 = VERTEX_POINT('',#22105) ;
#6243 = VERTEX_POINT('',#22107) ;
#6244 = VERTEX_POINT('',#22109) ;
#6245 = VERTEX_POINT('',#22114) ;
#6246 = VERTEX_POINT('',#22123) ;
#6247 = VERTEX_POINT('',#22125) ;
#6248 = VERTEX_POINT('',#22127) ;
#6249 = VERTEX_POINT('',#22131) ;
#6250 = VERTEX_POINT('',#22133) ;
#6251 = VERTEX_POINT('',#22135) ;
#6252 = VERTEX_POINT('',#22137) ;
#6253 = VERTEX_POINT('',#22142) ;
#6254 = VERTEX_POINT('',#22151) ;
#6255 = VERTEX_POINT('',#22153) ;
#6256 = VERTEX_POINT('',#22155) ;
#6257 = VERTEX_POINT('',#22159) ;
#6258 = VERTEX_POINT('',#22161) ;
#6259 = VERTEX_POINT('',#22163) ;
#6260 = VERTEX_POINT('',#22165) ;
#6261 = VERTEX_POINT('',#22170) ;
#6262 = VERTEX_POINT('',#22173) ;
#6263 = VERTEX_POINT('',#22179) ;
#6264 = VERTEX_POINT('',#22190) ;
#6265 = VERTEX_POINT('',#22196) ;
#6266 = VERTEX_POINT('',#22200) ;
#6267 = VERTEX_POINT('',#22204) ;
#6268 = VERTEX_POINT('',#22208) ;
#6269 = VERTEX_POINT('',#22210) ;
#6270 = VERTEX_POINT('',#22213) ;
#6271 = VERTEX_POINT('',#22216) ;
#6272 = VERTEX_POINT('',#22218) ;
#6273 = VERTEX_POINT('',#22221) ;
#6274 = VERTEX_POINT('',#22224) ;
#6275 = VERTEX_POINT('',#22226) ;
#6276 = VERTEX_POINT('',#22229) ;
#6277 = VERTEX_POINT('',#22232) ;
#6278 = VERTEX_POINT('',#22234) ;
#6279 = VERTEX_POINT('',#22237) ;
#6280 = VERTEX_POINT('',#22241) ;
#6281 = VERTEX_POINT('',#22242) ;
#6282 = VERTEX_POINT('',#22244) ;
#6283 = VERTEX_POINT('',#22246) ;
#6284 = VERTEX_POINT('',#22250) ;
#6285 = VERTEX_POINT('',#22252) ;
#6286 = VERTEX_POINT('',#22256) ;
#6287 = VERTEX_POINT('',#22258) ;
#6288 = VERTEX_POINT('',#22265) ;
#6289 = VERTEX_POINT('',#22267) ;
#6290 = VERTEX_POINT('',#22271) ;
#6291 = VERTEX_POINT('',#22272) ;
#6292 = VERTEX_POINT('',#22274) ;
#6293 = VERTEX_POINT('',#22276) ;
#6294 = VERTEX_POINT('',#22280) ;
#6295 = VERTEX_POINT('',#22282) ;
#6296 = VERTEX_POINT('',#22286) ;
#6297 = VERTEX_POINT('',#22288) ;
#6298 = VERTEX_POINT('',#22295) ;
#6299 = VERTEX_POINT('',#22297) ;
#6300 = VERTEX_POINT('',#22301) ;
#6301 = VERTEX_POINT('',#22302) ;
#6302 = VERTEX_POINT('',#22304) ;
#6303 = VERTEX_POINT('',#22306) ;
#6304 = VERTEX_POINT('',#22310) ;
#6305 = VERTEX_POINT('',#22312) ;
#6306 = VERTEX_POINT('',#22316) ;
#6307 = VERTEX_POINT('',#22318) ;
#6308 = VERTEX_POINT('',#22322) ;
#6309 = VERTEX_POINT('',#22323) ;
#6310 = VERTEX_POINT('',#22328) ;
#6311 = VERTEX_POINT('',#22332) ;
#6312 = VERTEX_POINT('',#22404) ;
#6313 = VERTEX_POINT('',#22405) ;
#6314 = VERTEX_POINT('',#22412) ;
#6315 = VERTEX_POINT('',#22429) ;
#6316 = VERTEX_POINT('',#22437) ;
#6317 = VERTEX_POINT('',#22448) ;
#6318 = VERTEX_POINT('',#22524) ;
#6319 = VERTEX_POINT('',#22531) ;
#6320 = VERTEX_POINT('',#22548) ;
#6321 = VERTEX_POINT('',#22604) ;
#6322 = VERTEX_POINT('',#22611) ;
#6323 = VERTEX_POINT('',#22628) ;
#6324 = VERTEX_POINT('',#22714) ;
#6325 = VERTEX_POINT('',#22715) ;
#6326 = VERTEX_POINT('',#22717) ;
#6327 = VERTEX_POINT('',#22719) ;
#6328 = VERTEX_POINT('',#22723) ;
#6329 = VERTEX_POINT('',#22724) ;
#6330 = VERTEX_POINT('',#22726) ;
#6331 = VERTEX_POINT('',#22728) ;
#6332 = VERTEX_POINT('',#22841) ;
#6333 = VERTEX_POINT('',#22843) ;
#6334 = VERTEX_POINT('',#22848) ;
#6335 = VERTEX_POINT('',#22849) ;
#6336 = VERTEX_POINT('',#22851) ;
#6337 = VERTEX_POINT('',#22853) ;
#6338 = VERTEX_POINT('',#22857) ;
#6339 = VERTEX_POINT('',#22859) ;
#6340 = VERTEX_POINT('',#22863) ;
#6341 = VERTEX_POINT('',#22867) ;
#6342 = VERTEX_POINT('',#22873) ;
#6343 = VERTEX_POINT('',#22874) ;
#6344 = VERTEX_POINT('',#22876) ;
#6345 = VERTEX_POINT('',#22878) ;
#6346 = VERTEX_POINT('',#22882) ;
#6347 = VERTEX_POINT('',#22884) ;
#6348 = VERTEX_POINT('',#22888) ;
#6349 = VERTEX_POINT('',#22892) ;
#6350 = VERTEX_POINT('',#22898) ;
#6351 = VERTEX_POINT('',#22899) ;
#6352 = VERTEX_POINT('',#22901) ;
#6353 = VERTEX_POINT('',#22903) ;
#6354 = VERTEX_POINT('',#22907) ;
#6355 = VERTEX_POINT('',#22908) ;
#6356 = VERTEX_POINT('',#22910) ;
#6357 = VERTEX_POINT('',#22912) ;
#6358 = VERTEX_POINT('',#22925) ;
#6359 = VERTEX_POINT('',#22926) ;
#6360 = VERTEX_POINT('',#22928) ;
#6361 = VERTEX_POINT('',#22930) ;
#6362 = VERTEX_POINT('',#22932) ;
#6363 = VERTEX_POINT('',#22934) ;
#6364 = VERTEX_POINT('',#22936) ;
#6365 = VERTEX_POINT('',#22938) ;
#6366 = VERTEX_POINT('',#22942) ;
#6367 = VERTEX_POINT('',#22943) ;
#6368 = VERTEX_POINT('',#22945) ;
#6369 = VERTEX_POINT('',#22947) ;
#6370 = VERTEX_POINT('',#22951) ;
#6371 = VERTEX_POINT('',#22953) ;
#6372 = VERTEX_POINT('',#22955) ;
#6373 = VERTEX_POINT('',#22957) ;
#6374 = VERTEX_POINT('',#22961) ;
#6375 = VERTEX_POINT('',#22963) ;
#6376 = VERTEX_POINT('',#22965) ;
#6377 = VERTEX_POINT('',#22967) ;
#6378 = VERTEX_POINT('',#22971) ;
#6379 = VERTEX_POINT('',#22972) ;
#6380 = VERTEX_POINT('',#22975) ;
#6381 = VERTEX_POINT('',#22977) ;
#6382 = VERTEX_POINT('',#22981) ;
#6383 = VERTEX_POINT('',#22987) ;
#6384 = VERTEX_POINT('',#22991) ;
#6385 = VERTEX_POINT('',#22995) ;
#6386 = VERTEX_POINT('',#22999) ;
#6387 = VERTEX_POINT('',#23001) ;
#6388 = VERTEX_POINT('',#23005) ;
#6389 = VERTEX_POINT('',#23007) ;
#6390 = VERTEX_POINT('',#23011) ;
#6391 = VERTEX_POINT('',#23015) ;
#6392 = VERTEX_POINT('',#23019) ;
#6393 = VERTEX_POINT('',#23023) ;
#6394 = VERTEX_POINT('',#23029) ;
#6395 = VERTEX_POINT('',#23031) ;
#6396 = VERTEX_POINT('',#23033) ;
#6397 = VERTEX_POINT('',#23087) ;
#6398 = VERTEX_POINT('',#23089) ;
#6399 = VERTEX_POINT('',#23093) ;
#6400 = VERTEX_POINT('',#23095) ;
#6401 = VERTEX_POINT('',#23099) ;
#6402 = VERTEX_POINT('',#23101) ;
#6403 = VERTEX_POINT('',#23104) ;
#6404 = VERTEX_POINT('',#23147) ;
#6405 = VERTEX_POINT('',#23151) ;
#6406 = VERTEX_POINT('',#23152) ;
#6407 = VERTEX_POINT('',#23154) ;
#6408 = VERTEX_POINT('',#23156) ;
#6409 = VERTEX_POINT('',#23160) ;
#6410 = VERTEX_POINT('',#23161) ;
#6411 = VERTEX_POINT('',#23163) ;
#6412 = VERTEX_POINT('',#23165) ;
#6413 = VERTEX_POINT('',#23178) ;
#6414 = VERTEX_POINT('',#23180) ;
#6415 = VERTEX_POINT('',#23184) ;
#6416 = VERTEX_POINT('',#23185) ;
#6417 = VERTEX_POINT('',#23187) ;
#6418 = VERTEX_POINT('',#23189) ;
#6419 = VERTEX_POINT('',#23193) ;
#6420 = VERTEX_POINT('',#23195) ;
#6421 = VERTEX_POINT('',#23197) ;
#6422 = VERTEX_POINT('',#23199) ;
#6423 = VERTEX_POINT('',#23201) ;
#6424 = VERTEX_POINT('',#23203) ;
#6425 = VERTEX_POINT('',#23205) ;
#6426 = VERTEX_POINT('',#23207) ;
#6427 = VERTEX_POINT('',#23209) ;
#6428 = VERTEX_POINT('',#23211) ;
#6429 = VERTEX_POINT('',#23213) ;
#6430 = VERTEX_POINT('',#23215) ;
#6431 = VERTEX_POINT('',#23217) ;
#6432 = VERTEX_POINT('',#23219) ;
#6433 = VERTEX_POINT('',#23223) ;
#6434 = VERTEX_POINT('',#23227) ;
#6435 = VERTEX_POINT('',#23231) ;
#6436 = VERTEX_POINT('',#23235) ;
#6437 = VERTEX_POINT('',#23239) ;
#6438 = VERTEX_POINT('',#23243) ;
#6439 = VERTEX_POINT('',#23247) ;
#6440 = VERTEX_POINT('',#23251) ;
#6441 = VERTEX_POINT('',#23255) ;
#6442 = VERTEX_POINT('',#23259) ;
#6443 = VERTEX_POINT('',#23263) ;
#6444 = VERTEX_POINT('',#23267) ;
#6445 = VERTEX_POINT('',#23271) ;
#6446 = VERTEX_POINT('',#23275) ;
#6447 = VERTEX_POINT('',#23283) ;
#6448 = VERTEX_POINT('',#23285) ;
#6449 = VERTEX_POINT('',#23292) ;
#6450 = VERTEX_POINT('',#23294) ;
#6451 = VERTEX_POINT('',#23298) ;
#6452 = VERTEX_POINT('',#23300) ;
#6453 = VERTEX_POINT('',#23307) ;
#6454 = VERTEX_POINT('',#23309) ;
#6455 = VERTEX_POINT('',#23313) ;
#6456 = VERTEX_POINT('',#23315) ;
#6457 = VERTEX_POINT('',#23320) ;
#6458 = VERTEX_POINT('',#23321) ;
#6459 = VERTEX_POINT('',#23323) ;
#6460 = VERTEX_POINT('',#23325) ;
#6461 = VERTEX_POINT('',#23329) ;
#6462 = VERTEX_POINT('',#23331) ;
#6463 = VERTEX_POINT('',#23335) ;
#6464 = VERTEX_POINT('',#23337) ;
#6465 = VERTEX_POINT('',#23345) ;
#6466 = VERTEX_POINT('',#23346) ;
#6467 = VERTEX_POINT('',#23348) ;
#6468 = VERTEX_POINT('',#23350) ;
#6469 = VERTEX_POINT('',#23354) ;
#6470 = VERTEX_POINT('',#23356) ;
#6471 = VERTEX_POINT('',#23360) ;
#6472 = VERTEX_POINT('',#23362) ;
#6473 = VERTEX_POINT('',#23370) ;
#6474 = VERTEX_POINT('',#23371) ;
#6475 = VERTEX_POINT('',#23373) ;
#6476 = VERTEX_POINT('',#23375) ;
#6477 = VERTEX_POINT('',#23379) ;
#6478 = VERTEX_POINT('',#23381) ;
#6479 = VERTEX_POINT('',#23385) ;
#6480 = VERTEX_POINT('',#23387) ;
#6481 = VERTEX_POINT('',#23395) ;
#6482 = VERTEX_POINT('',#23396) ;
#6483 = VERTEX_POINT('',#23398) ;
#6484 = VERTEX_POINT('',#23400) ;
#6485 = VERTEX_POINT('',#23404) ;
#6486 = VERTEX_POINT('',#23406) ;
#6487 = VERTEX_POINT('',#23410) ;
#6488 = VERTEX_POINT('',#23412) ;
#6489 = VERTEX_POINT('',#23420) ;
#6490 = VERTEX_POINT('',#23421) ;
#6491 = VERTEX_POINT('',#23423) ;
#6492 = VERTEX_POINT('',#23425) ;
#6493 = VERTEX_POINT('',#23427) ;
#6494 = VERTEX_POINT('',#23431) ;
#6495 = VERTEX_POINT('',#23433) ;
#6496 = VERTEX_POINT('',#23437) ;
#6497 = VERTEX_POINT('',#23439) ;
#6498 = VERTEX_POINT('',#23443) ;
#6499 = VERTEX_POINT('',#23449) ;
#6500 = VERTEX_POINT('',#23450) ;
#6501 = VERTEX_POINT('',#23452) ;
#6502 = VERTEX_POINT('',#23454) ;
#6503 = VERTEX_POINT('',#23458) ;
#6504 = VERTEX_POINT('',#23460) ;
#6505 = VERTEX_POINT('',#23464) ;
#6506 = VERTEX_POINT('',#23466) ;
#6507 = VERTEX_POINT('',#23474) ;
#6508 = VERTEX_POINT('',#23475) ;
#6509 = VERTEX_POINT('',#23477) ;
#6510 = VERTEX_POINT('',#23479) ;
#6511 = VERTEX_POINT('',#23483) ;
#6512 = VERTEX_POINT('',#23485) ;
#6513 = VERTEX_POINT('',#23489) ;
#6514 = VERTEX_POINT('',#23491) ;
#6515 = VERTEX_POINT('',#23499) ;
#6516 = VERTEX_POINT('',#23500) ;
#6517 = VERTEX_POINT('',#23502) ;
#6518 = VERTEX_POINT('',#23504) ;
#6519 = VERTEX_POINT('',#23508) ;
#6520 = VERTEX_POINT('',#23510) ;
#6521 = VERTEX_POINT('',#23514) ;
#6522 = VERTEX_POINT('',#23516) ;
#6523 = VERTEX_POINT('',#23524) ;
#6524 = VERTEX_POINT('',#23525) ;
#6525 = VERTEX_POINT('',#23527) ;
#6526 = VERTEX_POINT('',#23529) ;
#6527 = VERTEX_POINT('',#23533) ;
#6528 = VERTEX_POINT('',#23535) ;
#6529 = VERTEX_POINT('',#23539) ;
#6530 = VERTEX_POINT('',#23541) ;
#6531 = VERTEX_POINT('',#23549) ;
#6532 = VERTEX_POINT('',#23550) ;
#6533 = VERTEX_POINT('',#23552) ;
#6534 = VERTEX_POINT('',#23554) ;
#6535 = VERTEX_POINT('',#23558) ;
#6536 = VERTEX_POINT('',#23560) ;
#6537 = VERTEX_POINT('',#23564) ;
#6538 = VERTEX_POINT('',#23566) ;
#6539 = VERTEX_POINT('',#23574) ;
#6540 = VERTEX_POINT('',#23577) ;
#6541 = VERTEX_POINT('',#23584) ;
#6542 = VERTEX_POINT('',#23586) ;
#6543 = VERTEX_POINT('',#23590) ;
#6544 = VERTEX_POINT('',#23592) ;
#6545 = VERTEX_POINT('',#23599) ;
#6546 = VERTEX_POINT('',#23600) ;
#6547 = VERTEX_POINT('',#23602) ;
#6548 = VERTEX_POINT('',#23604) ;
#6549 = VERTEX_POINT('',#23608) ;
#6550 = VERTEX_POINT('',#23613) ;
#6551 = VERTEX_POINT('',#23615) ;
#6552 = VERTEX_POINT('',#23617) ;
#6553 = VERTEX_POINT('',#23653) ;
#6554 = VERTEX_POINT('',#23655) ;
#6555 = VERTEX_POINT('',#23657) ;
#6556 = VERTEX_POINT('',#23663) ;
#6557 = VERTEX_POINT('',#23668) ;
#6558 = VERTEX_POINT('',#23669) ;
#6559 = VERTEX_POINT('',#23671) ;
#6560 = VERTEX_POINT('',#23673) ;
#6561 = VERTEX_POINT('',#23675) ;
#6562 = VERTEX_POINT('',#23679) ;
#6563 = VERTEX_POINT('',#23680) ;
#6564 = VERTEX_POINT('',#23685) ;
#6565 = VERTEX_POINT('',#23693) ;
#6566 = VERTEX_POINT('',#23697) ;
#6567 = VERTEX_POINT('',#23703) ;
#6568 = VERTEX_POINT('',#23704) ;
#6569 = VERTEX_POINT('',#23706) ;
#6570 = VERTEX_POINT('',#23708) ;
#6571 = VERTEX_POINT('',#23712) ;
#6572 = VERTEX_POINT('',#23713) ;
#6573 = VERTEX_POINT('',#23715) ;
#6574 = VERTEX_POINT('',#23717) ;
#6575 = VERTEX_POINT('',#23721) ;
#6576 = VERTEX_POINT('',#23722) ;
#6577 = VERTEX_POINT('',#23724) ;
#6578 = VERTEX_POINT('',#23726) ;
#6579 = VERTEX_POINT('',#23742) ;
#6580 = VERTEX_POINT('',#23743) ;
#6581 = VERTEX_POINT('',#23745) ;
#6582 = VERTEX_POINT('',#23747) ;
#6583 = VERTEX_POINT('',#23751) ;
#6584 = VERTEX_POINT('',#23752) ;
#6585 = VERTEX_POINT('',#23754) ;
#6586 = VERTEX_POINT('',#23756) ;
#6587 = VERTEX_POINT('',#23760) ;
#6588 = VERTEX_POINT('',#23761) ;
#6589 = VERTEX_POINT('',#23763) ;
#6590 = VERTEX_POINT('',#23765) ;
#6591 = VERTEX_POINT('',#23794) ;
#6592 = VERTEX_POINT('',#23795) ;
#6593 = VERTEX_POINT('',#23810) ;
#6594 = VERTEX_POINT('',#23825) ;
#6595 = VERTEX_POINT('',#23827) ;
#6596 = VERTEX_POINT('',#23842) ;
#6597 = VERTEX_POINT('',#23910) ;
#6598 = VERTEX_POINT('',#23913) ;
#6599 = VERTEX_POINT('',#23917) ;
#6600 = VERTEX_POINT('',#23920) ;
#6601 = VERTEX_POINT('',#23927) ;
#6602 = VERTEX_POINT('',#23928) ;
#6603 = VERTEX_POINT('',#23930) ;
#6604 = VERTEX_POINT('',#23932) ;
#6605 = VERTEX_POINT('',#23936) ;
#6606 = VERTEX_POINT('',#23950) ;
#6607 = VERTEX_POINT('',#23968) ;
#6608 = VERTEX_POINT('',#23985) ;
#6609 = VERTEX_POINT('',#24000) ;
#6610 = VERTEX_POINT('',#24001) ;
#6611 = VERTEX_POINT('',#24014) ;
#6612 = VERTEX_POINT('',#24016) ;
#6613 = VERTEX_POINT('',#24067) ;
#6614 = VERTEX_POINT('',#24070) ;
#6615 = VERTEX_POINT('',#24074) ;
#6616 = VERTEX_POINT('',#24076) ;
#6617 = VERTEX_POINT('',#24082) ;
#6618 = VERTEX_POINT('',#24086) ;
#6619 = VERTEX_POINT('',#24092) ;
#6620 = VERTEX_POINT('',#24094) ;
#6621 = VERTEX_POINT('',#24098) ;
#6622 = VERTEX_POINT('',#24100) ;
#6623 = VERTEX_POINT('',#24107) ;
#6624 = VERTEX_POINT('',#24109) ;
#6625 = VERTEX_POINT('',#24113) ;
#6626 = VERTEX_POINT('',#24115) ;
#6627 = VERTEX_POINT('',#24119) ;
#6628 = VERTEX_POINT('',#24121) ;
#6629 = VERTEX_POINT('',#24125) ;
#6630 = VERTEX_POINT('',#24127) ;
#6631 = VERTEX_POINT('',#24131) ;
#6632 = VERTEX_POINT('',#24133) ;
#6633 = VERTEX_POINT('',#24137) ;
#6634 = VERTEX_POINT('',#24139) ;
#6635 = VERTEX_POINT('',#24146) ;
#6636 = VERTEX_POINT('',#24148) ;
#6637 = VERTEX_POINT('',#24152) ;
#6638 = VERTEX_POINT('',#24154) ;
#6639 = VERTEX_POINT('',#24158) ;
#6640 = VERTEX_POINT('',#24160) ;
#6641 = VERTEX_POINT('',#24164) ;
#6642 = VERTEX_POINT('',#24166) ;
#6643 = VERTEX_POINT('',#24170) ;
#6644 = VERTEX_POINT('',#24172) ;
#6645 = VERTEX_POINT('',#24176) ;
#6646 = VERTEX_POINT('',#24178) ;
#6647 = VERTEX_POINT('',#24185) ;
#6648 = VERTEX_POINT('',#24186) ;
#6649 = VERTEX_POINT('',#24190) ;
#6650 = VERTEX_POINT('',#24192) ;
#6651 = VERTEX_POINT('',#24216) ;
#6652 = VERTEX_POINT('',#24217) ;
#6653 = VERTEX_POINT('',#24221) ;
#6654 = VERTEX_POINT('',#24223) ;
#6655 = VERTEX_POINT('',#24246) ;
#6656 = VERTEX_POINT('',#24247) ;
#6657 = VERTEX_POINT('',#24249) ;
#6658 = VERTEX_POINT('',#24251) ;
#6659 = VERTEX_POINT('',#24255) ;
#6660 = VERTEX_POINT('',#24256) ;
#6661 = VERTEX_POINT('',#24258) ;
#6662 = VERTEX_POINT('',#24260) ;
#6663 = VERTEX_POINT('',#24264) ;
#6664 = VERTEX_POINT('',#24265) ;
#6665 = VERTEX_POINT('',#24267) ;
#6666 = VERTEX_POINT('',#24269) ;
#6667 = VERTEX_POINT('',#24280) ;
#6668 = VERTEX_POINT('',#24285) ;
#6669 = VERTEX_POINT('',#24299) ;
#6670 = VERTEX_POINT('',#24301) ;
#6671 = VERTEX_POINT('',#24306) ;
#6672 = VERTEX_POINT('',#24308) ;
#6673 = VERTEX_POINT('',#24315) ;
#6674 = VERTEX_POINT('',#24317) ;
#6675 = VERTEX_POINT('',#24321) ;
#6676 = VERTEX_POINT('',#24323) ;
#6677 = VERTEX_POINT('',#24330) ;
#6678 = VERTEX_POINT('',#24332) ;
#6679 = VERTEX_POINT('',#24336) ;
#6680 = VERTEX_POINT('',#24337) ;
#6681 = VERTEX_POINT('',#24339) ;
#6682 = VERTEX_POINT('',#24341) ;
#6683 = VERTEX_POINT('',#24345) ;
#6684 = VERTEX_POINT('',#24346) ;
#6685 = VERTEX_POINT('',#24348) ;
#6686 = VERTEX_POINT('',#24350) ;
#6687 = VERTEX_POINT('',#24354) ;
#6688 = VERTEX_POINT('',#24357) ;
#6689 = VERTEX_POINT('',#24361) ;
#6690 = VERTEX_POINT('',#24365) ;
#6691 = VERTEX_POINT('',#24375) ;
#6692 = VERTEX_POINT('',#24377) ;
#6693 = VERTEX_POINT('',#24382) ;
#6694 = VERTEX_POINT('',#24383) ;
#6695 = VERTEX_POINT('',#24385) ;
#6696 = VERTEX_POINT('',#24387) ;
#6697 = VERTEX_POINT('',#24391) ;
#6698 = VERTEX_POINT('',#24392) ;
#6699 = VERTEX_POINT('',#24394) ;
#6700 = VERTEX_POINT('',#24396) ;
#6701 = VERTEX_POINT('',#24400) ;
#6702 = VERTEX_POINT('',#24403) ;
#6703 = VERTEX_POINT('',#24407) ;
#6704 = VERTEX_POINT('',#24411) ;
#6705 = VERTEX_POINT('',#24421) ;
#6706 = VERTEX_POINT('',#24423) ;
#6707 = VERTEX_POINT('',#24428) ;
#6708 = VERTEX_POINT('',#24429) ;
#6709 = VERTEX_POINT('',#24431) ;
#6710 = VERTEX_POINT('',#24433) ;
#6711 = VERTEX_POINT('',#24437) ;
#6712 = VERTEX_POINT('',#24438) ;
#6713 = VERTEX_POINT('',#24440) ;
#6714 = VERTEX_POINT('',#24442) ;
#6715 = VERTEX_POINT('',#24446) ;
#6716 = VERTEX_POINT('',#24449) ;
#6717 = VERTEX_POINT('',#24453) ;
#6718 = VERTEX_POINT('',#24457) ;
#6719 = VERTEX_POINT('',#24467) ;
#6720 = VERTEX_POINT('',#24469) ;
#6721 = VERTEX_POINT('',#24473) ;
#6722 = VERTEX_POINT('',#24474) ;
#6723 = VERTEX_POINT('',#24476) ;
#6724 = VERTEX_POINT('',#24478) ;
#6725 = VERTEX_POINT('',#24482) ;
#6726 = VERTEX_POINT('',#24483) ;
#6727 = VERTEX_POINT('',#24485) ;
#6728 = VERTEX_POINT('',#24487) ;
#6729 = VERTEX_POINT('',#24491) ;
#6730 = VERTEX_POINT('',#24494) ;
#6731 = VERTEX_POINT('',#24498) ;
#6732 = VERTEX_POINT('',#24502) ;
#6733 = EDGE_CURVE('',#5537,#5538,#4751,.T.) ;
#6734 = EDGE_CURVE('',#5539,#5537,#4752,.T.) ;
#6735 = EDGE_CURVE('',#5538,#5539,#4753,.T.) ;
#6736 = EDGE_CURVE('',#5540,#5540,#4754,.T.) ;
#6737 = EDGE_CURVE('',#5540,#5539,#1001,.T.) ;
#6738 = EDGE_CURVE('',#5541,#5537,#1002,.T.) ;
#6739 = EDGE_CURVE('',#5542,#5541,#4755,.T.) ;
#6740 = EDGE_CURVE('',#5538,#5542,#1003,.T.) ;
#6741 = EDGE_CURVE('',#5542,#5543,#4756,.T.) ;
#6742 = EDGE_CURVE('',#5543,#5544,#1004,.T.) ;
#6743 = EDGE_CURVE('',#5544,#5545,#4757,.T.) ;
#6744 = EDGE_CURVE('',#5545,#5546,#1005,.T.) ;
#6745 = EDGE_CURVE('',#5546,#5547,#4758,.T.) ;
#6746 = EDGE_CURVE('',#5547,#5548,#1006,.T.) ;
#6747 = EDGE_CURVE('',#5548,#5548,#4759,.T.) ;
#6748 = EDGE_CURVE('',#5547,#5549,#4760,.T.) ;
#6749 = EDGE_CURVE('',#5549,#5550,#1007,.T.) ;
#6750 = EDGE_CURVE('',#5550,#5551,#4761,.T.) ;
#6751 = EDGE_CURVE('',#5551,#5552,#1008,.T.) ;
#6752 = EDGE_CURVE('',#5552,#5541,#4762,.T.) ;
#6753 = EDGE_CURVE('',#5553,#5554,#951,.T.) ;
#6754 = EDGE_CURVE('',#5554,#5555,#952,.T.) ;
#6755 = EDGE_CURVE('',#5555,#5556,#1009,.T.) ;
#6756 = EDGE_CURVE('',#5556,#5557,#953,.T.) ;
#6757 = EDGE_CURVE('',#5557,#5553,#1010,.T.) ;
#6758 = EDGE_CURVE('',#5558,#5558,#4763,.T.) ;
#6759 = EDGE_CURVE('',#5558,#5559,#1011,.T.) ;
#6760 = EDGE_CURVE('',#5559,#5544,#4764,.T.) ;
#6761 = EDGE_CURVE('',#5546,#5543,#4765,.T.) ;
#6762 = EDGE_CURVE('',#5545,#5559,#4766,.T.) ;
#6763 = EDGE_CURVE('',#5552,#5560,#4767,.T.) ;
#6764 = EDGE_CURVE('',#5560,#5549,#4768,.T.) ;
#6765 = EDGE_CURVE('',#5561,#5561,#4769,.T.) ;
#6766 = EDGE_CURVE('',#5562,#5562,#4770,.T.) ;
#6767 = EDGE_CURVE('',#5562,#5563,#1012,.T.) ;
#6768 = EDGE_CURVE('',#5563,#5563,#4771,.T.) ;
#6769 = EDGE_CURVE('',#5564,#5564,#4772,.T.) ;
#6770 = EDGE_CURVE('',#5564,#5565,#1013,.T.) ;
#6771 = EDGE_CURVE('',#5565,#5565,#4773,.T.) ;
#6772 = EDGE_CURVE('',#5566,#5566,#4774,.T.) ;
#6773 = EDGE_CURVE('',#5566,#5567,#1014,.T.) ;
#6774 = EDGE_CURVE('',#5567,#5567,#4775,.T.) ;
#6775 = EDGE_CURVE('',#5568,#5568,#4776,.T.) ;
#6776 = EDGE_CURVE('',#5568,#5569,#1015,.T.) ;
#6777 = EDGE_CURVE('',#5569,#5569,#4777,.T.) ;
#6778 = EDGE_CURVE('',#5570,#5570,#4778,.T.) ;
#6779 = EDGE_CURVE('',#5570,#5571,#1016,.T.) ;
#6780 = EDGE_CURVE('',#5571,#5571,#4779,.T.) ;
#6781 = EDGE_CURVE('',#5572,#5572,#4780,.T.) ;
#6782 = EDGE_CURVE('',#5572,#5573,#1017,.T.) ;
#6783 = EDGE_CURVE('',#5573,#5573,#4781,.T.) ;
#6784 = EDGE_CURVE('',#5574,#5575,#1018,.T.) ;
#6785 = EDGE_CURVE('',#5576,#5574,#1019,.T.) ;
#6786 = EDGE_CURVE('',#5577,#5576,#1020,.T.) ;
#6787 = EDGE_CURVE('',#5578,#5577,#1021,.T.) ;
#6788 = EDGE_CURVE('',#5579,#5578,#1022,.T.) ;
#6789 = EDGE_CURVE('',#5579,#5575,#1023,.T.) ;
#6790 = EDGE_CURVE('',#5580,#5576,#1024,.T.) ;
#6791 = EDGE_CURVE('',#5580,#5581,#1025,.T.) ;
#6792 = EDGE_CURVE('',#5581,#5577,#1026,.T.) ;
#6793 = EDGE_CURVE('',#5575,#5582,#4782,.T.) ;
#6794 = EDGE_CURVE('',#5582,#5579,#1027,.T.) ;
#6795 = EDGE_CURVE('',#5583,#5584,#1028,.T.) ;
#6796 = EDGE_CURVE('',#5584,#5582,#1029,.T.) ;
#6797 = EDGE_CURVE('',#5578,#5583,#1030,.T.) ;
#6798 = EDGE_CURVE('',#5583,#5581,#1031,.T.) ;
#6799 = EDGE_CURVE('',#5582,#5585,#4783,.T.) ;
#6800 = EDGE_CURVE('',#5584,#5585,#1032,.T.) ;
#6801 = EDGE_CURVE('',#5585,#5586,#1033,.T.) ;
#6802 = EDGE_CURVE('',#5586,#5580,#1034,.T.) ;
#6803 = EDGE_CURVE('',#5587,#5587,#4784,.T.) ;
#6804 = EDGE_CURVE('',#5587,#5588,#1035,.T.) ;
#6805 = EDGE_CURVE('',#5574,#5588,#4785,.T.) ;
#6806 = EDGE_CURVE('',#5589,#5586,#4786,.T.) ;
#6807 = EDGE_CURVE('',#5589,#5590,#1036,.T.) ;
#6808 = EDGE_CURVE('',#5590,#5591,#4787,.T.) ;
#6809 = EDGE_CURVE('',#5591,#5592,#1037,.T.) ;
#6810 = EDGE_CURVE('',#5588,#5592,#4788,.T.) ;
#6811 = EDGE_CURVE('',#5593,#5594,#954,.T.) ;
#6812 = EDGE_CURVE('',#5594,#5593,#955,.T.) ;
#6813 = EDGE_CURVE('',#5595,#5595,#4789,.T.) ;
#6814 = EDGE_CURVE('',#5595,#5554,#1038,.T.) ;
#6815 = EDGE_CURVE('',#5555,#5553,#4790,.T.) ;
#6816 = EDGE_CURVE('',#5594,#5596,#1039,.T.) ;
#6817 = EDGE_CURVE('',#5596,#5596,#4791,.T.) ;
#6818 = EDGE_CURVE('',#5557,#5556,#4792,.T.) ;
#6819 = EDGE_CURVE('',#5551,#5550,#4793,.T.) ;
#6820 = EDGE_CURVE('',#5597,#5597,#4794,.T.) ;
#6821 = EDGE_CURVE('',#5597,#5560,#1040,.T.) ;
#6822 = EDGE_CURVE('',#5590,#5591,#4795,.T.) ;
#6823 = EDGE_CURVE('',#5598,#5589,#4796,.T.) ;
#6824 = EDGE_CURVE('',#5598,#5599,#1041,.T.) ;
#6825 = EDGE_CURVE('',#5599,#5599,#4797,.T.) ;
#6826 = EDGE_CURVE('',#5592,#5598,#4798,.T.) ;
#6827 = EDGE_CURVE('',#5600,#5600,#4799,.T.) ;
#6828 = EDGE_CURVE('',#5601,#5601,#4800,.T.) ;
#6829 = EDGE_CURVE('',#5601,#5602,#1042,.T.) ;
#6830 = EDGE_CURVE('',#5602,#5602,#4801,.T.) ;
#6831 = EDGE_CURVE('',#5603,#5603,#4802,.T.) ;
#6832 = EDGE_CURVE('',#5603,#5604,#1043,.T.) ;
#6833 = EDGE_CURVE('',#5604,#5604,#4803,.T.) ;
#6834 = EDGE_CURVE('',#5605,#5605,#4804,.T.) ;
#6835 = EDGE_CURVE('',#5605,#5606,#1044,.T.) ;
#6836 = EDGE_CURVE('',#5606,#5606,#4805,.T.) ;
#6837 = EDGE_CURVE('',#5607,#5607,#4806,.T.) ;
#6838 = EDGE_CURVE('',#5607,#5561,#1045,.T.) ;
#6839 = EDGE_CURVE('',#5600,#5608,#1046,.T.) ;
#6840 = EDGE_CURVE('',#5608,#5608,#4807,.T.) ;
#6841 = EDGE_CURVE('',#5609,#5609,#4808,.T.) ;
#6842 = EDGE_CURVE('',#5609,#5610,#1047,.T.) ;
#6843 = EDGE_CURVE('',#5610,#5610,#4809,.T.) ;
#6844 = EDGE_CURVE('',#5611,#5611,#4810,.T.) ;
#6845 = EDGE_CURVE('',#5611,#5612,#1048,.T.) ;
#6846 = EDGE_CURVE('',#5612,#5612,#4811,.T.) ;
#6847 = EDGE_CURVE('',#5613,#5613,#4812,.T.) ;
#6848 = EDGE_CURVE('',#5613,#5614,#1049,.T.) ;
#6849 = EDGE_CURVE('',#5614,#5614,#4813,.T.) ;
#6850 = EDGE_CURVE('',#5615,#5615,#4814,.T.) ;
#6851 = EDGE_CURVE('',#5615,#5616,#1050,.T.) ;
#6852 = EDGE_CURVE('',#5616,#5616,#4815,.T.) ;
#6853 = EDGE_CURVE('',#5617,#5617,#4816,.T.) ;
#6854 = EDGE_CURVE('',#5617,#5618,#1051,.T.) ;
#6855 = EDGE_CURVE('',#5618,#5618,#4817,.T.) ;
#6856 = EDGE_CURVE('',#5619,#5619,#4818,.T.) ;
#6857 = EDGE_CURVE('',#5619,#5620,#1052,.T.) ;
#6858 = EDGE_CURVE('',#5620,#5620,#4819,.T.) ;
#6859 = EDGE_CURVE('',#5621,#5621,#4820,.T.) ;
#6860 = EDGE_CURVE('',#5621,#5622,#1053,.T.) ;
#6861 = EDGE_CURVE('',#5622,#5622,#4821,.T.) ;
#6862 = EDGE_CURVE('',#5623,#5623,#4822,.T.) ;
#6863 = EDGE_CURVE('',#5623,#5624,#1054,.T.) ;
#6864 = EDGE_CURVE('',#5624,#5624,#4823,.T.) ;
#6865 = EDGE_CURVE('',#5625,#5625,#4824,.T.) ;
#6866 = EDGE_CURVE('',#5625,#5626,#1055,.T.) ;
#6867 = EDGE_CURVE('',#5626,#5626,#4825,.T.) ;
#6868 = EDGE_CURVE('',#5627,#5627,#4826,.T.) ;
#6869 = EDGE_CURVE('',#5627,#5628,#1056,.T.) ;
#6870 = EDGE_CURVE('',#5628,#5628,#4827,.T.) ;
#6871 = EDGE_CURVE('',#5629,#5629,#4828,.T.) ;
#6872 = EDGE_CURVE('',#5629,#5630,#1057,.T.) ;
#6873 = EDGE_CURVE('',#5630,#5630,#4829,.T.) ;
#6874 = EDGE_CURVE('',#5631,#5631,#4830,.T.) ;
#6875 = EDGE_CURVE('',#5631,#5632,#1058,.T.) ;
#6876 = EDGE_CURVE('',#5632,#5632,#4831,.T.) ;
#6877 = EDGE_CURVE('',#5633,#5633,#4832,.T.) ;
#6878 = EDGE_CURVE('',#5634,#5634,#4833,.T.) ;
#6879 = EDGE_CURVE('',#5634,#5633,#1059,.T.) ;
#6880 = EDGE_CURVE('',#5635,#5635,#4834,.T.) ;
#6881 = EDGE_CURVE('',#5635,#5636,#1060,.T.) ;
#6882 = EDGE_CURVE('',#5636,#5636,#4835,.T.) ;
#6883 = EDGE_CURVE('',#5637,#5637,#4836,.T.) ;
#6884 = EDGE_CURVE('',#5637,#5638,#1061,.T.) ;
#6885 = EDGE_CURVE('',#5638,#5638,#4837,.T.) ;
#6886 = EDGE_CURVE('',#5639,#5639,#4838,.T.) ;
#6887 = EDGE_CURVE('',#5639,#5640,#1062,.T.) ;
#6888 = EDGE_CURVE('',#5640,#5640,#4839,.T.) ;
#6889 = EDGE_CURVE('',#5641,#5641,#4840,.T.) ;
#6890 = EDGE_CURVE('',#5641,#5642,#1063,.T.) ;
#6891 = EDGE_CURVE('',#5642,#5642,#4841,.T.) ;
#6892 = EDGE_CURVE('',#5643,#5643,#4842,.T.) ;
#6893 = EDGE_CURVE('',#5643,#5644,#1064,.T.) ;
#6894 = EDGE_CURVE('',#5644,#5644,#4843,.T.) ;
#6895 = EDGE_CURVE('',#5645,#5645,#4844,.T.) ;
#6896 = EDGE_CURVE('',#5645,#5646,#1065,.T.) ;
#6897 = EDGE_CURVE('',#5646,#5646,#4845,.T.) ;
#6898 = EDGE_CURVE('',#5647,#5647,#4846,.T.) ;
#6899 = EDGE_CURVE('',#5647,#5648,#1066,.T.) ;
#6900 = EDGE_CURVE('',#5648,#5648,#4847,.T.) ;
#6901 = EDGE_CURVE('',#5649,#5649,#4848,.T.) ;
#6902 = EDGE_CURVE('',#5649,#5650,#1067,.T.) ;
#6903 = EDGE_CURVE('',#5650,#5650,#4849,.T.) ;
#6904 = EDGE_CURVE('',#5651,#5651,#4850,.T.) ;
#6905 = EDGE_CURVE('',#5651,#5652,#1068,.T.) ;
#6906 = EDGE_CURVE('',#5652,#5652,#4851,.T.) ;
#6907 = EDGE_CURVE('',#5653,#5653,#4852,.T.) ;
#6908 = EDGE_CURVE('',#5653,#5654,#1069,.T.) ;
#6909 = EDGE_CURVE('',#5654,#5654,#4853,.T.) ;
#6910 = EDGE_CURVE('',#5655,#5655,#4854,.T.) ;
#6911 = EDGE_CURVE('',#5655,#5656,#1070,.T.) ;
#6912 = EDGE_CURVE('',#5656,#5656,#4855,.T.) ;
#6913 = EDGE_CURVE('',#5657,#5658,#1071,.T.) ;
#6914 = EDGE_CURVE('',#5659,#5657,#1072,.T.) ;
#6915 = EDGE_CURVE('',#5660,#5659,#1073,.T.) ;
#6916 = EDGE_CURVE('',#5658,#5660,#1074,.T.) ;
#6917 = EDGE_CURVE('',#5660,#5661,#4856,.T.) ;
#6918 = EDGE_CURVE('',#5659,#5662,#1075,.T.) ;
#6919 = EDGE_CURVE('',#5662,#5661,#1076,.T.) ;
#6920 = EDGE_CURVE('',#5663,#5664,#1077,.T.) ;
#6921 = EDGE_CURVE('',#5661,#5663,#1078,.T.) ;
#6922 = EDGE_CURVE('',#5664,#5662,#1079,.T.) ;
#6923 = EDGE_CURVE('',#5664,#5657,#1080,.T.) ;
#6924 = EDGE_CURVE('',#5665,#5665,#4857,.T.) ;
#6925 = EDGE_CURVE('',#5665,#5666,#1081,.T.) ;
#6926 = EDGE_CURVE('',#5658,#5666,#4858,.T.) ;
#6927 = EDGE_CURVE('',#5666,#5663,#4859,.T.) ;
#6928 = EDGE_CURVE('',#5667,#5667,#4860,.T.) ;
#6929 = EDGE_CURVE('',#5667,#5668,#1082,.T.) ;
#6930 = EDGE_CURVE('',#5668,#5668,#4861,.T.) ;
#6931 = EDGE_CURVE('',#5669,#5669,#4862,.T.) ;
#6932 = EDGE_CURVE('',#5670,#5670,#4863,.T.) ;
#6933 = EDGE_CURVE('',#5670,#5669,#1083,.T.) ;
#6934 = EDGE_CURVE('',#5671,#5671,#4864,.T.) ;
#6935 = EDGE_CURVE('',#5671,#5672,#1084,.T.) ;
#6936 = EDGE_CURVE('',#5672,#5672,#4865,.T.) ;
#6937 = EDGE_CURVE('',#5673,#5673,#4866,.T.) ;
#6938 = EDGE_CURVE('',#5673,#5674,#1085,.T.) ;
#6939 = EDGE_CURVE('',#5674,#5674,#4867,.T.) ;
#6940 = EDGE_CURVE('',#5675,#5675,#4868,.T.) ;
#6941 = EDGE_CURVE('',#5675,#5676,#1086,.T.) ;
#6942 = EDGE_CURVE('',#5676,#5676,#4869,.T.) ;
#6943 = EDGE_CURVE('',#5677,#5677,#4870,.T.) ;
#6944 = EDGE_CURVE('',#5678,#5678,#4871,.T.) ;
#6945 = EDGE_CURVE('',#5678,#5677,#1087,.T.) ;
#6946 = EDGE_CURVE('',#5679,#5679,#4872,.T.) ;
#6947 = EDGE_CURVE('',#5679,#5680,#1088,.T.) ;
#6948 = EDGE_CURVE('',#5680,#5680,#4873,.T.) ;
#6949 = EDGE_CURVE('',#5681,#5681,#4874,.T.) ;
#6950 = EDGE_CURVE('',#5681,#5682,#1089,.T.) ;
#6951 = EDGE_CURVE('',#5682,#5682,#4875,.T.) ;
#6952 = EDGE_CURVE('',#5683,#5683,#4876,.T.) ;
#6953 = EDGE_CURVE('',#5683,#5684,#1090,.T.) ;
#6954 = EDGE_CURVE('',#5684,#5684,#4877,.T.) ;
#6955 = EDGE_CURVE('',#5685,#5685,#4878,.T.) ;
#6956 = EDGE_CURVE('',#5685,#5686,#1091,.T.) ;
#6957 = EDGE_CURVE('',#5686,#5686,#4879,.T.) ;
#6958 = EDGE_CURVE('',#5687,#5687,#4880,.T.) ;
#6959 = EDGE_CURVE('',#5687,#5688,#1092,.T.) ;
#6960 = EDGE_CURVE('',#5688,#5688,#4881,.T.) ;
#6961 = EDGE_CURVE('',#5689,#5689,#4882,.T.) ;
#6962 = EDGE_CURVE('',#5689,#5690,#1093,.T.) ;
#6963 = EDGE_CURVE('',#5690,#5690,#4883,.T.) ;
#6964 = EDGE_CURVE('',#5691,#5691,#4884,.T.) ;
#6965 = EDGE_CURVE('',#5691,#5692,#1094,.T.) ;
#6966 = EDGE_CURVE('',#5692,#5692,#4885,.T.) ;
#6967 = EDGE_CURVE('',#5693,#5693,#4886,.T.) ;
#6968 = EDGE_CURVE('',#5693,#5694,#1095,.T.) ;
#6969 = EDGE_CURVE('',#5694,#5694,#4887,.T.) ;
#6970 = EDGE_CURVE('',#5695,#5695,#4888,.T.) ;
#6971 = EDGE_CURVE('',#5695,#5696,#1096,.T.) ;
#6972 = EDGE_CURVE('',#5696,#5696,#4889,.T.) ;
#6973 = EDGE_CURVE('',#5697,#5697,#4890,.T.) ;
#6974 = EDGE_CURVE('',#5697,#5698,#1097,.T.) ;
#6975 = EDGE_CURVE('',#5698,#5698,#4891,.T.) ;
#6976 = EDGE_CURVE('',#5699,#5699,#4892,.T.) ;
#6977 = EDGE_CURVE('',#5699,#5700,#1098,.T.) ;
#6978 = EDGE_CURVE('',#5700,#5700,#4893,.T.) ;
#6979 = EDGE_CURVE('',#5701,#5701,#4894,.T.) ;
#6980 = EDGE_CURVE('',#5701,#5702,#1099,.T.) ;
#6981 = EDGE_CURVE('',#5702,#5702,#4895,.T.) ;
#6982 = EDGE_CURVE('',#5703,#5703,#4896,.T.) ;
#6983 = EDGE_CURVE('',#5703,#5704,#1100,.T.) ;
#6984 = EDGE_CURVE('',#5704,#5704,#4897,.T.) ;
#6985 = EDGE_CURVE('',#5705,#5705,#4898,.T.) ;
#6986 = EDGE_CURVE('',#5705,#5706,#1101,.T.) ;
#6987 = EDGE_CURVE('',#5706,#5706,#4899,.T.) ;
#6988 = EDGE_CURVE('',#5707,#5707,#4900,.T.) ;
#6989 = EDGE_CURVE('',#5707,#5708,#1102,.T.) ;
#6990 = EDGE_CURVE('',#5708,#5708,#4901,.T.) ;
#6991 = EDGE_CURVE('',#5709,#5709,#4902,.T.) ;
#6992 = EDGE_CURVE('',#5709,#5710,#1103,.T.) ;
#6993 = EDGE_CURVE('',#5710,#5710,#4903,.T.) ;
#6994 = EDGE_CURVE('',#5711,#5711,#4904,.T.) ;
#6995 = EDGE_CURVE('',#5711,#5712,#1104,.T.) ;
#6996 = EDGE_CURVE('',#5712,#5712,#4905,.T.) ;
#6997 = EDGE_CURVE('',#5713,#5713,#4906,.T.) ;
#6998 = EDGE_CURVE('',#5713,#5714,#1105,.T.) ;
#6999 = EDGE_CURVE('',#5714,#5714,#4907,.T.) ;
#7000 = EDGE_CURVE('',#5715,#5715,#4908,.T.) ;
#7001 = EDGE_CURVE('',#5715,#5716,#1106,.T.) ;
#7002 = EDGE_CURVE('',#5716,#5716,#4909,.T.) ;
#7003 = EDGE_CURVE('',#5717,#5717,#4910,.T.) ;
#7004 = EDGE_CURVE('',#5717,#5718,#1107,.T.) ;
#7005 = EDGE_CURVE('',#5718,#5718,#4911,.T.) ;
#7006 = EDGE_CURVE('',#5719,#5719,#4912,.T.) ;
#7007 = EDGE_CURVE('',#5719,#5720,#1108,.T.) ;
#7008 = EDGE_CURVE('',#5720,#5720,#4913,.T.) ;
#7009 = EDGE_CURVE('',#5721,#5721,#4914,.T.) ;
#7010 = EDGE_CURVE('',#5721,#5722,#1109,.T.) ;
#7011 = EDGE_CURVE('',#5722,#5722,#4915,.T.) ;
#7012 = EDGE_CURVE('',#5723,#5723,#4916,.T.) ;
#7013 = EDGE_CURVE('',#5723,#5724,#1110,.T.) ;
#7014 = EDGE_CURVE('',#5724,#5724,#4917,.T.) ;
#7015 = EDGE_CURVE('',#5725,#5725,#4918,.T.) ;
#7016 = EDGE_CURVE('',#5725,#5726,#1111,.T.) ;
#7017 = EDGE_CURVE('',#5726,#5726,#4919,.T.) ;
#7018 = EDGE_CURVE('',#5727,#5727,#4920,.T.) ;
#7019 = EDGE_CURVE('',#5727,#5728,#1112,.T.) ;
#7020 = EDGE_CURVE('',#5728,#5728,#4921,.T.) ;
#7021 = EDGE_CURVE('',#5729,#5729,#4922,.T.) ;
#7022 = EDGE_CURVE('',#5729,#5730,#1113,.T.) ;
#7023 = EDGE_CURVE('',#5730,#5730,#4923,.T.) ;
#7024 = EDGE_CURVE('',#5731,#5731,#4924,.T.) ;
#7025 = EDGE_CURVE('',#5731,#5732,#1114,.T.) ;
#7026 = EDGE_CURVE('',#5732,#5732,#4925,.T.) ;
#7027 = EDGE_CURVE('',#5733,#5733,#4926,.T.) ;
#7028 = EDGE_CURVE('',#5733,#5734,#1115,.T.) ;
#7029 = EDGE_CURVE('',#5734,#5734,#4927,.T.) ;
#7030 = EDGE_CURVE('',#5735,#5735,#4928,.T.) ;
#7031 = EDGE_CURVE('',#5735,#5736,#1116,.T.) ;
#7032 = EDGE_CURVE('',#5736,#5736,#4929,.T.) ;
#7033 = EDGE_CURVE('',#5737,#5737,#4930,.T.) ;
#7034 = EDGE_CURVE('',#5737,#5738,#1117,.T.) ;
#7035 = EDGE_CURVE('',#5738,#5738,#4931,.T.) ;
#7036 = EDGE_CURVE('',#5739,#5739,#4932,.T.) ;
#7037 = EDGE_CURVE('',#5739,#5740,#1118,.T.) ;
#7038 = EDGE_CURVE('',#5740,#5740,#4933,.T.) ;
#7039 = EDGE_CURVE('',#5741,#5741,#4934,.T.) ;
#7040 = EDGE_CURVE('',#5741,#5742,#1119,.T.) ;
#7041 = EDGE_CURVE('',#5742,#5742,#4935,.T.) ;
#7042 = EDGE_CURVE('',#5743,#5743,#4936,.T.) ;
#7043 = EDGE_CURVE('',#5743,#5744,#1120,.T.) ;
#7044 = EDGE_CURVE('',#5744,#5744,#4937,.T.) ;
#7045 = EDGE_CURVE('',#5745,#5745,#4938,.T.) ;
#7046 = EDGE_CURVE('',#5745,#5746,#1121,.T.) ;
#7047 = EDGE_CURVE('',#5746,#5746,#4939,.T.) ;
#7048 = EDGE_CURVE('',#5747,#5747,#4940,.T.) ;
#7049 = EDGE_CURVE('',#5747,#5748,#1122,.T.) ;
#7050 = EDGE_CURVE('',#5748,#5748,#4941,.T.) ;
#7051 = EDGE_CURVE('',#5749,#5749,#4942,.T.) ;
#7052 = EDGE_CURVE('',#5749,#5750,#1123,.T.) ;
#7053 = EDGE_CURVE('',#5750,#5750,#4943,.T.) ;
#7054 = EDGE_CURVE('',#5751,#5751,#4944,.T.) ;
#7055 = EDGE_CURVE('',#5751,#5752,#1124,.T.) ;
#7056 = EDGE_CURVE('',#5752,#5752,#4945,.T.) ;
#7057 = EDGE_CURVE('',#5753,#5753,#4946,.T.) ;
#7058 = EDGE_CURVE('',#5753,#5754,#1125,.T.) ;
#7059 = EDGE_CURVE('',#5754,#5754,#4947,.T.) ;
#7060 = EDGE_CURVE('',#5755,#5755,#4948,.T.) ;
#7061 = EDGE_CURVE('',#5755,#5756,#1126,.T.) ;
#7062 = EDGE_CURVE('',#5756,#5756,#4949,.T.) ;
#7063 = EDGE_CURVE('',#5757,#5757,#4950,.T.) ;
#7064 = EDGE_CURVE('',#5757,#5758,#1127,.T.) ;
#7065 = EDGE_CURVE('',#5758,#5758,#4951,.T.) ;
#7066 = EDGE_CURVE('',#5759,#5759,#4952,.T.) ;
#7067 = EDGE_CURVE('',#5759,#5760,#1128,.T.) ;
#7068 = EDGE_CURVE('',#5760,#5760,#4953,.T.) ;
#7069 = EDGE_CURVE('',#5761,#5761,#4954,.T.) ;
#7070 = EDGE_CURVE('',#5761,#5762,#1129,.T.) ;
#7071 = EDGE_CURVE('',#5762,#5762,#4955,.T.) ;
#7072 = EDGE_CURVE('',#5763,#5763,#4956,.T.) ;
#7073 = EDGE_CURVE('',#5763,#5764,#1130,.T.) ;
#7074 = EDGE_CURVE('',#5764,#5764,#4957,.T.) ;
#7075 = EDGE_CURVE('',#5765,#5765,#4958,.T.) ;
#7076 = EDGE_CURVE('',#5765,#5766,#1131,.T.) ;
#7077 = EDGE_CURVE('',#5766,#5766,#4959,.T.) ;
#7078 = EDGE_CURVE('',#5767,#5767,#4960,.T.) ;
#7079 = EDGE_CURVE('',#5767,#5768,#1132,.T.) ;
#7080 = EDGE_CURVE('',#5768,#5768,#4961,.T.) ;
#7081 = EDGE_CURVE('',#5769,#5769,#4962,.T.) ;
#7082 = EDGE_CURVE('',#5769,#5770,#1133,.T.) ;
#7083 = EDGE_CURVE('',#5770,#5770,#4963,.T.) ;
#7084 = EDGE_CURVE('',#5771,#5771,#4964,.T.) ;
#7085 = EDGE_CURVE('',#5771,#5772,#1134,.T.) ;
#7086 = EDGE_CURVE('',#5772,#5772,#4965,.T.) ;
#7087 = EDGE_CURVE('',#5773,#5773,#4966,.T.) ;
#7088 = EDGE_CURVE('',#5773,#5774,#1135,.T.) ;
#7089 = EDGE_CURVE('',#5774,#5774,#4967,.T.) ;
#7090 = EDGE_CURVE('',#5775,#5775,#4968,.T.) ;
#7091 = EDGE_CURVE('',#5775,#5776,#1136,.T.) ;
#7092 = EDGE_CURVE('',#5776,#5776,#4969,.T.) ;
#7093 = EDGE_CURVE('',#5777,#5777,#4970,.T.) ;
#7094 = EDGE_CURVE('',#5777,#5778,#1137,.T.) ;
#7095 = EDGE_CURVE('',#5778,#5778,#4971,.T.) ;
#7096 = EDGE_CURVE('',#5779,#5779,#4972,.T.) ;
#7097 = EDGE_CURVE('',#5779,#5780,#1138,.T.) ;
#7098 = EDGE_CURVE('',#5780,#5780,#4973,.T.) ;
#7099 = EDGE_CURVE('',#5781,#5781,#4974,.T.) ;
#7100 = EDGE_CURVE('',#5781,#5782,#1139,.T.) ;
#7101 = EDGE_CURVE('',#5782,#5782,#4975,.T.) ;
#7102 = EDGE_CURVE('',#5783,#5783,#4976,.T.) ;
#7103 = EDGE_CURVE('',#5783,#5784,#1140,.T.) ;
#7104 = EDGE_CURVE('',#5784,#5784,#4977,.T.) ;
#7105 = EDGE_CURVE('',#5785,#5785,#4978,.T.) ;
#7106 = EDGE_CURVE('',#5785,#5786,#1141,.T.) ;
#7107 = EDGE_CURVE('',#5786,#5786,#4979,.T.) ;
#7108 = EDGE_CURVE('',#5787,#5787,#4980,.T.) ;
#7109 = EDGE_CURVE('',#5788,#5788,#4981,.T.) ;
#7110 = EDGE_CURVE('',#5789,#5789,#4982,.T.) ;
#7111 = EDGE_CURVE('',#5790,#5790,#4983,.T.) ;
#7112 = EDGE_CURVE('',#5788,#5790,#1142,.T.) ;
#7113 = EDGE_CURVE('',#5789,#5787,#1143,.T.) ;
#7114 = EDGE_CURVE('',#5791,#5791,#4984,.T.) ;
#7115 = EDGE_CURVE('',#5792,#5792,#4985,.T.) ;
#7116 = EDGE_CURVE('',#5793,#5793,#4986,.T.) ;
#7117 = EDGE_CURVE('',#5793,#5791,#1144,.T.) ;
#7118 = EDGE_CURVE('',#5794,#5794,#4987,.T.) ;
#7119 = EDGE_CURVE('',#5792,#5794,#1145,.T.) ;
#7120 = EDGE_CURVE('',#5795,#5795,#4988,.T.) ;
#7121 = EDGE_CURVE('',#5796,#5796,#4989,.T.) ;
#7122 = EDGE_CURVE('',#5797,#5797,#4990,.T.) ;
#7123 = EDGE_CURVE('',#5798,#5798,#4991,.T.) ;
#7124 = EDGE_CURVE('',#5796,#5798,#1146,.T.) ;
#7125 = EDGE_CURVE('',#5797,#5795,#1147,.T.) ;
#7126 = EDGE_CURVE('',#5799,#5799,#4992,.T.) ;
#7127 = EDGE_CURVE('',#5800,#5800,#4993,.T.) ;
#7128 = EDGE_CURVE('',#5801,#5801,#4994,.T.) ;
#7129 = EDGE_CURVE('',#5801,#5799,#1148,.T.) ;
#7130 = EDGE_CURVE('',#5802,#5802,#4995,.T.) ;
#7131 = EDGE_CURVE('',#5800,#5802,#1149,.T.) ;
#7132 = EDGE_CURVE('',#5803,#5803,#4996,.T.) ;
#7133 = EDGE_CURVE('',#5803,#5804,#1150,.T.) ;
#7134 = EDGE_CURVE('',#5804,#5804,#4997,.T.) ;
#7135 = EDGE_CURVE('',#5805,#5805,#4998,.T.) ;
#7136 = EDGE_CURVE('',#5805,#5806,#1151,.T.) ;
#7137 = EDGE_CURVE('',#5806,#5806,#4999,.T.) ;
#7138 = EDGE_CURVE('',#5807,#5808,#1152,.T.) ;
#7139 = EDGE_CURVE('',#5809,#5807,#1153,.T.) ;
#7140 = EDGE_CURVE('',#5810,#5809,#1154,.T.) ;
#7141 = EDGE_CURVE('',#5808,#5810,#1155,.T.) ;
#7142 = EDGE_CURVE('',#5811,#5812,#1156,.T.) ;
#7143 = EDGE_CURVE('',#5813,#5811,#1157,.T.) ;
#7144 = EDGE_CURVE('',#5814,#5813,#1158,.T.) ;
#7145 = EDGE_CURVE('',#5812,#5814,#1159,.T.) ;
#7146 = EDGE_CURVE('',#5807,#5812,#5000,.T.) ;
#7147 = EDGE_CURVE('',#5814,#5809,#5001,.T.) ;
#7148 = EDGE_CURVE('',#5810,#5813,#5002,.T.) ;
#7149 = EDGE_CURVE('',#5811,#5808,#5003,.T.) ;
#7150 = EDGE_CURVE('',#5815,#5816,#1160,.T.) ;
#7151 = EDGE_CURVE('',#5817,#5815,#1161,.T.) ;
#7152 = EDGE_CURVE('',#5818,#5817,#1162,.T.) ;
#7153 = EDGE_CURVE('',#5816,#5818,#1163,.T.) ;
#7154 = EDGE_CURVE('',#5819,#5820,#1164,.T.) ;
#7155 = EDGE_CURVE('',#5821,#5819,#1165,.T.) ;
#7156 = EDGE_CURVE('',#5822,#5821,#1166,.T.) ;
#7157 = EDGE_CURVE('',#5820,#5822,#1167,.T.) ;
#7158 = EDGE_CURVE('',#5820,#5815,#1168,.T.) ;
#7159 = EDGE_CURVE('',#5817,#5822,#1169,.T.) ;
#7160 = EDGE_CURVE('',#5823,#5823,#5004,.T.) ;
#7161 = EDGE_CURVE('',#5821,#5818,#5005,.T.) ;
#7162 = EDGE_CURVE('',#5816,#5819,#5006,.T.) ;
#7163 = EDGE_CURVE('',#5824,#5825,#1170,.T.) ;
#7164 = EDGE_CURVE('',#5824,#5826,#1171,.T.) ;
#7165 = EDGE_CURVE('',#5826,#5827,#1172,.T.) ;
#7166 = EDGE_CURVE('',#5827,#5825,#1173,.T.) ;
#7167 = EDGE_CURVE('',#5828,#5829,#1174,.T.) ;
#7168 = EDGE_CURVE('',#5828,#5830,#1175,.T.) ;
#7169 = EDGE_CURVE('',#5830,#5831,#1176,.T.) ;
#7170 = EDGE_CURVE('',#5831,#5829,#1177,.T.) ;
#7171 = EDGE_CURVE('',#5830,#5827,#1178,.T.) ;
#7172 = EDGE_CURVE('',#5831,#5826,#1179,.T.) ;
#7173 = EDGE_CURVE('',#5832,#5825,#5007,.T.) ;
#7174 = EDGE_CURVE('',#5832,#5833,#1180,.T.) ;
#7175 = EDGE_CURVE('',#5824,#5833,#5008,.T.) ;
#7176 = EDGE_CURVE('',#5834,#5829,#5009,.T.) ;
#7177 = EDGE_CURVE('',#5834,#5835,#1181,.T.) ;
#7178 = EDGE_CURVE('',#5828,#5835,#5010,.T.) ;
#7179 = EDGE_CURVE('',#5836,#5833,#1182,.T.) ;
#7180 = EDGE_CURVE('',#5836,#5837,#1183,.T.) ;
#7181 = EDGE_CURVE('',#5838,#5837,#1184,.T.) ;
#7182 = EDGE_CURVE('',#5838,#5839,#5011,.T.) ;
#7183 = EDGE_CURVE('',#5840,#5839,#1185,.T.) ;
#7184 = EDGE_CURVE('',#5840,#5841,#1186,.T.) ;
#7185 = EDGE_CURVE('',#5842,#5841,#1187,.T.) ;
#7186 = EDGE_CURVE('',#5842,#5843,#5012,.T.) ;
#7187 = EDGE_CURVE('',#5844,#5843,#1188,.T.) ;
#7188 = EDGE_CURVE('',#5844,#5845,#1189,.T.) ;
#7189 = EDGE_CURVE('',#5846,#5845,#1190,.T.) ;
#7190 = EDGE_CURVE('',#5846,#5847,#5013,.T.) ;
#7191 = EDGE_CURVE('',#5848,#5847,#1191,.T.) ;
#7192 = EDGE_CURVE('',#5848,#5849,#1192,.T.) ;
#7193 = EDGE_CURVE('',#5850,#5849,#1193,.T.) ;
#7194 = EDGE_CURVE('',#5850,#5851,#5014,.T.) ;
#7195 = EDGE_CURVE('',#5852,#5851,#1194,.T.) ;
#7196 = EDGE_CURVE('',#5852,#5853,#1195,.T.) ;
#7197 = EDGE_CURVE('',#5854,#5853,#1196,.T.) ;
#7198 = EDGE_CURVE('',#5854,#5855,#5015,.T.) ;
#7199 = EDGE_CURVE('',#5856,#5855,#1197,.T.) ;
#7200 = EDGE_CURVE('',#5856,#5857,#1198,.T.) ;
#7201 = EDGE_CURVE('',#5858,#5857,#1199,.T.) ;
#7202 = EDGE_CURVE('',#5858,#5859,#5016,.T.) ;
#7203 = EDGE_CURVE('',#5860,#5859,#1200,.T.) ;
#7204 = EDGE_CURVE('',#5860,#5861,#1201,.T.) ;
#7205 = EDGE_CURVE('',#5862,#5861,#1202,.T.) ;
#7206 = EDGE_CURVE('',#5862,#5863,#5017,.T.) ;
#7207 = EDGE_CURVE('',#5864,#5863,#1203,.T.) ;
#7208 = EDGE_CURVE('',#5864,#5865,#1204,.T.) ;
#7209 = EDGE_CURVE('',#5866,#5865,#1205,.T.) ;
#7210 = EDGE_CURVE('',#5866,#5867,#5018,.T.) ;
#7211 = EDGE_CURVE('',#5868,#5867,#1206,.T.) ;
#7212 = EDGE_CURVE('',#5868,#5869,#1207,.T.) ;
#7213 = EDGE_CURVE('',#5870,#5869,#1208,.T.) ;
#7214 = EDGE_CURVE('',#5870,#5871,#5019,.T.) ;
#7215 = EDGE_CURVE('',#5872,#5871,#1209,.T.) ;
#7216 = EDGE_CURVE('',#5872,#5873,#1210,.T.) ;
#7217 = EDGE_CURVE('',#5874,#5873,#1211,.T.) ;
#7218 = EDGE_CURVE('',#5874,#5875,#5020,.T.) ;
#7219 = EDGE_CURVE('',#5876,#5875,#1212,.T.) ;
#7220 = EDGE_CURVE('',#5876,#5877,#1213,.T.) ;
#7221 = EDGE_CURVE('',#5834,#5877,#1214,.T.) ;
#7222 = EDGE_CURVE('',#5832,#5878,#1215,.T.) ;
#7223 = EDGE_CURVE('',#5878,#5836,#1216,.T.) ;
#7224 = EDGE_CURVE('',#5838,#5879,#1217,.T.) ;
#7225 = EDGE_CURVE('',#5837,#5880,#1218,.T.) ;
#7226 = EDGE_CURVE('',#5880,#5879,#1219,.T.) ;
#7227 = EDGE_CURVE('',#5878,#5880,#1220,.T.) ;
#7228 = EDGE_CURVE('',#5881,#5879,#5021,.T.) ;
#7229 = EDGE_CURVE('',#5881,#5839,#1221,.T.) ;
#7230 = EDGE_CURVE('',#5842,#5882,#1222,.T.) ;
#7231 = EDGE_CURVE('',#5841,#5883,#1223,.T.) ;
#7232 = EDGE_CURVE('',#5883,#5882,#1224,.T.) ;
#7233 = EDGE_CURVE('',#5881,#5884,#1225,.T.) ;
#7234 = EDGE_CURVE('',#5884,#5840,#1226,.T.) ;
#7235 = EDGE_CURVE('',#5884,#5883,#1227,.T.) ;
#7236 = EDGE_CURVE('',#5885,#5882,#5022,.T.) ;
#7237 = EDGE_CURVE('',#5885,#5843,#1228,.T.) ;
#7238 = EDGE_CURVE('',#5885,#5886,#1229,.T.) ;
#7239 = EDGE_CURVE('',#5886,#5844,#1230,.T.) ;
#7240 = EDGE_CURVE('',#5846,#5887,#1231,.T.) ;
#7241 = EDGE_CURVE('',#5845,#5888,#1232,.T.) ;
#7242 = EDGE_CURVE('',#5888,#5887,#1233,.T.) ;
#7243 = EDGE_CURVE('',#5886,#5888,#1234,.T.) ;
#7244 = EDGE_CURVE('',#5889,#5887,#5023,.T.) ;
#7245 = EDGE_CURVE('',#5889,#5847,#1235,.T.) ;
#7246 = EDGE_CURVE('',#5850,#5890,#1236,.T.) ;
#7247 = EDGE_CURVE('',#5849,#5891,#1237,.T.) ;
#7248 = EDGE_CURVE('',#5891,#5890,#1238,.T.) ;
#7249 = EDGE_CURVE('',#5889,#5892,#1239,.T.) ;
#7250 = EDGE_CURVE('',#5892,#5848,#1240,.T.) ;
#7251 = EDGE_CURVE('',#5892,#5891,#1241,.T.) ;
#7252 = EDGE_CURVE('',#5893,#5890,#5024,.T.) ;
#7253 = EDGE_CURVE('',#5893,#5851,#1242,.T.) ;
#7254 = EDGE_CURVE('',#5893,#5894,#1243,.T.) ;
#7255 = EDGE_CURVE('',#5894,#5852,#1244,.T.) ;
#7256 = EDGE_CURVE('',#5854,#5895,#1245,.T.) ;
#7257 = EDGE_CURVE('',#5853,#5896,#1246,.T.) ;
#7258 = EDGE_CURVE('',#5896,#5895,#1247,.T.) ;
#7259 = EDGE_CURVE('',#5894,#5896,#1248,.T.) ;
#7260 = EDGE_CURVE('',#5897,#5895,#5025,.T.) ;
#7261 = EDGE_CURVE('',#5897,#5855,#1249,.T.) ;
#7262 = EDGE_CURVE('',#5858,#5898,#1250,.T.) ;
#7263 = EDGE_CURVE('',#5857,#5899,#1251,.T.) ;
#7264 = EDGE_CURVE('',#5899,#5898,#1252,.T.) ;
#7265 = EDGE_CURVE('',#5897,#5900,#1253,.T.) ;
#7266 = EDGE_CURVE('',#5900,#5856,#1254,.T.) ;
#7267 = EDGE_CURVE('',#5900,#5899,#1255,.T.) ;
#7268 = EDGE_CURVE('',#5901,#5898,#5026,.T.) ;
#7269 = EDGE_CURVE('',#5901,#5859,#1256,.T.) ;
#7270 = EDGE_CURVE('',#5901,#5902,#1257,.T.) ;
#7271 = EDGE_CURVE('',#5902,#5860,#1258,.T.) ;
#7272 = EDGE_CURVE('',#5862,#5903,#1259,.T.) ;
#7273 = EDGE_CURVE('',#5861,#5904,#1260,.T.) ;
#7274 = EDGE_CURVE('',#5904,#5903,#1261,.T.) ;
#7275 = EDGE_CURVE('',#5902,#5904,#1262,.T.) ;
#7276 = EDGE_CURVE('',#5905,#5903,#5027,.T.) ;
#7277 = EDGE_CURVE('',#5905,#5863,#1263,.T.) ;
#7278 = EDGE_CURVE('',#5866,#5906,#1264,.T.) ;
#7279 = EDGE_CURVE('',#5865,#5907,#1265,.T.) ;
#7280 = EDGE_CURVE('',#5907,#5906,#1266,.T.) ;
#7281 = EDGE_CURVE('',#5905,#5908,#1267,.T.) ;
#7282 = EDGE_CURVE('',#5908,#5864,#1268,.T.) ;
#7283 = EDGE_CURVE('',#5908,#5907,#1269,.T.) ;
#7284 = EDGE_CURVE('',#5909,#5906,#5028,.T.) ;
#7285 = EDGE_CURVE('',#5909,#5867,#1270,.T.) ;
#7286 = EDGE_CURVE('',#5909,#5910,#1271,.T.) ;
#7287 = EDGE_CURVE('',#5910,#5868,#1272,.T.) ;
#7288 = EDGE_CURVE('',#5870,#5911,#1273,.T.) ;
#7289 = EDGE_CURVE('',#5869,#5912,#1274,.T.) ;
#7290 = EDGE_CURVE('',#5912,#5911,#1275,.T.) ;
#7291 = EDGE_CURVE('',#5910,#5912,#1276,.T.) ;
#7292 = EDGE_CURVE('',#5913,#5911,#5029,.T.) ;
#7293 = EDGE_CURVE('',#5913,#5871,#1277,.T.) ;
#7294 = EDGE_CURVE('',#5874,#5914,#1278,.T.) ;
#7295 = EDGE_CURVE('',#5873,#5915,#1279,.T.) ;
#7296 = EDGE_CURVE('',#5915,#5914,#1280,.T.) ;
#7297 = EDGE_CURVE('',#5913,#5916,#1281,.T.) ;
#7298 = EDGE_CURVE('',#5916,#5872,#1282,.T.) ;
#7299 = EDGE_CURVE('',#5916,#5915,#1283,.T.) ;
#7300 = EDGE_CURVE('',#5917,#5914,#5030,.T.) ;
#7301 = EDGE_CURVE('',#5917,#5875,#1284,.T.) ;
#7302 = EDGE_CURVE('',#5917,#5918,#1285,.T.) ;
#7303 = EDGE_CURVE('',#5918,#5876,#1286,.T.) ;
#7304 = EDGE_CURVE('',#5877,#5919,#1287,.T.) ;
#7305 = EDGE_CURVE('',#5919,#5835,#1288,.T.) ;
#7306 = EDGE_CURVE('',#5918,#5919,#1289,.T.) ;
#7307 = EDGE_CURVE('',#5920,#5920,#5031,.T.) ;
#7308 = EDGE_CURVE('',#5920,#5823,#1290,.T.) ;
#7309 = EDGE_CURVE('',#5921,#5922,#1291,.T.) ;
#7310 = EDGE_CURVE('',#5922,#5923,#1292,.T.) ;
#7311 = EDGE_CURVE('',#5923,#5924,#1293,.T.) ;
#7312 = EDGE_CURVE('',#5924,#5921,#1294,.T.) ;
#7313 = EDGE_CURVE('',#5925,#5926,#1295,.T.) ;
#7314 = EDGE_CURVE('',#5926,#5927,#1296,.T.) ;
#7315 = EDGE_CURVE('',#5927,#5928,#1297,.T.) ;
#7316 = EDGE_CURVE('',#5928,#5925,#1298,.T.) ;
#7317 = EDGE_CURVE('',#5924,#5927,#1299,.T.) ;
#7318 = EDGE_CURVE('',#5921,#5926,#1300,.T.) ;
#7319 = EDGE_CURVE('',#5923,#5928,#1301,.T.) ;
#7320 = EDGE_CURVE('',#5922,#5925,#1302,.T.) ;
#7321 = EDGE_CURVE('',#5929,#5929,#5032,.T.) ;
#7322 = EDGE_CURVE('',#5929,#5930,#1303,.T.) ;
#7323 = EDGE_CURVE('',#5930,#5930,#5033,.T.) ;
#7324 = EDGE_CURVE('',#5931,#5931,#5034,.T.) ;
#7325 = EDGE_CURVE('',#5931,#5932,#1304,.T.) ;
#7326 = EDGE_CURVE('',#5932,#5932,#5035,.T.) ;
#7327 = EDGE_CURVE('',#5933,#5934,#1305,.T.) ;
#7328 = EDGE_CURVE('',#5935,#5933,#1306,.T.) ;
#7329 = EDGE_CURVE('',#5936,#5935,#1307,.T.) ;
#7330 = EDGE_CURVE('',#5934,#5936,#1308,.T.) ;
#7331 = EDGE_CURVE('',#5934,#5937,#1309,.T.) ;
#7332 = EDGE_CURVE('',#5938,#5936,#1310,.T.) ;
#7333 = EDGE_CURVE('',#5937,#5938,#1311,.T.) ;
#7334 = EDGE_CURVE('',#5938,#5939,#1312,.T.) ;
#7335 = EDGE_CURVE('',#5939,#5935,#1313,.T.) ;
#7336 = EDGE_CURVE('',#5940,#5933,#1314,.T.) ;
#7337 = EDGE_CURVE('',#5939,#5940,#1315,.T.) ;
#7338 = EDGE_CURVE('',#5941,#5937,#1316,.T.) ;
#7339 = EDGE_CURVE('',#5941,#5942,#1317,.T.) ;
#7340 = EDGE_CURVE('',#5943,#5942,#1318,.T.) ;
#7341 = EDGE_CURVE('',#5944,#5943,#1319,.T.) ;
#7342 = EDGE_CURVE('',#5940,#5944,#1320,.T.) ;
#7343 = EDGE_CURVE('',#5944,#5945,#1321,.T.) ;
#7344 = EDGE_CURVE('',#5945,#5946,#1322,.T.) ;
#7345 = EDGE_CURVE('',#5946,#5941,#1323,.T.) ;
#7346 = EDGE_CURVE('',#5942,#5947,#1324,.T.) ;
#7347 = EDGE_CURVE('',#5947,#5948,#1325,.T.) ;
#7348 = EDGE_CURVE('',#5948,#5943,#1326,.T.) ;
#7349 = EDGE_CURVE('',#5945,#5948,#1327,.T.) ;
#7350 = EDGE_CURVE('',#5946,#5947,#1328,.T.) ;
#7351 = EDGE_CURVE('',#5949,#5949,#5036,.T.) ;
#7352 = EDGE_CURVE('',#5949,#5950,#1329,.T.) ;
#7353 = EDGE_CURVE('',#5950,#5950,#5037,.T.) ;
#7354 = EDGE_CURVE('',#5951,#5951,#5038,.T.) ;
#7355 = EDGE_CURVE('',#5951,#5952,#1330,.T.) ;
#7356 = EDGE_CURVE('',#5952,#5952,#5039,.T.) ;
#7357 = EDGE_CURVE('',#5953,#5954,#1331,.T.) ;
#7358 = EDGE_CURVE('',#5955,#5953,#5040,.T.) ;
#7359 = EDGE_CURVE('',#5956,#5955,#1332,.T.) ;
#7360 = EDGE_CURVE('',#5954,#5956,#5041,.T.) ;
#7361 = EDGE_CURVE('',#5957,#5958,#1333,.T.) ;
#7362 = EDGE_CURVE('',#5959,#5957,#5042,.T.) ;
#7363 = EDGE_CURVE('',#5960,#5959,#1334,.T.) ;
#7364 = EDGE_CURVE('',#5958,#5960,#5043,.T.) ;
#7365 = EDGE_CURVE('',#5961,#5962,#1335,.T.) ;
#7366 = EDGE_CURVE('',#5963,#5961,#5044,.T.) ;
#7367 = EDGE_CURVE('',#5964,#5963,#1336,.T.) ;
#7368 = EDGE_CURVE('',#5962,#5964,#5045,.T.) ;
#7369 = EDGE_CURVE('',#5963,#5965,#1337,.T.) ;
#7370 = EDGE_CURVE('',#5965,#5966,#1338,.T.) ;
#7371 = EDGE_CURVE('',#5966,#5964,#1339,.T.) ;
#7372 = EDGE_CURVE('',#5962,#5967,#1340,.T.) ;
#7373 = EDGE_CURVE('',#5967,#5968,#1341,.T.) ;
#7374 = EDGE_CURVE('',#5968,#5961,#1342,.T.) ;
#7375 = EDGE_CURVE('',#5959,#5969,#1343,.T.) ;
#7376 = EDGE_CURVE('',#5970,#5969,#1344,.T.) ;
#7377 = EDGE_CURVE('',#5960,#5970,#1345,.T.) ;
#7378 = EDGE_CURVE('',#5967,#5957,#1346,.T.) ;
#7379 = EDGE_CURVE('',#5966,#5971,#1347,.T.) ;
#7380 = EDGE_CURVE('',#5954,#5971,#1348,.T.) ;
#7381 = EDGE_CURVE('',#5969,#5956,#1349,.T.) ;
#7382 = EDGE_CURVE('',#5955,#5970,#1350,.T.) ;
#7383 = EDGE_CURVE('',#5971,#5972,#1351,.T.) ;
#7384 = EDGE_CURVE('',#5972,#5953,#1352,.T.) ;
#7385 = EDGE_CURVE('',#5968,#5958,#1353,.T.) ;
#7386 = EDGE_CURVE('',#5965,#5972,#1354,.T.) ;
#7387 = EDGE_CURVE('',#5973,#5973,#5046,.T.) ;
#7388 = EDGE_CURVE('',#5973,#5974,#1355,.T.) ;
#7389 = EDGE_CURVE('',#5974,#5974,#5047,.T.) ;
#7390 = EDGE_CURVE('',#5975,#5976,#5048,.T.) ;
#7391 = EDGE_CURVE('',#5976,#5975,#5049,.T.) ;
#7392 = EDGE_CURVE('',#5977,#5978,#5050,.T.) ;
#7393 = EDGE_CURVE('',#5978,#5979,#5051,.T.) ;
#7394 = EDGE_CURVE('',#5979,#5980,#5052,.T.) ;
#7395 = EDGE_CURVE('',#5981,#5980,#5053,.T.) ;
#7396 = EDGE_CURVE('',#5980,#5977,#5054,.T.) ;
#7397 = EDGE_CURVE('',#5982,#5983,#5055,.T.) ;
#7398 = EDGE_CURVE('',#5983,#5984,#5056,.T.) ;
#7399 = EDGE_CURVE('',#5984,#5985,#5057,.T.) ;
#7400 = EDGE_CURVE('',#5985,#5982,#5058,.T.) ;
#7401 = EDGE_CURVE('',#5986,#5987,#5059,.T.) ;
#7402 = EDGE_CURVE('',#5987,#5988,#5060,.T.) ;
#7403 = EDGE_CURVE('',#5988,#5989,#5061,.T.) ;
#7404 = EDGE_CURVE('',#5989,#5986,#5062,.T.) ;
#7405 = EDGE_CURVE('',#5990,#5991,#5063,.T.) ;
#7406 = EDGE_CURVE('',#5991,#5992,#5064,.T.) ;
#7407 = EDGE_CURVE('',#5992,#5993,#5065,.T.) ;
#7408 = EDGE_CURVE('',#5993,#5990,#5066,.T.) ;
#7409 = EDGE_CURVE('',#5994,#5995,#5067,.T.) ;
#7410 = EDGE_CURVE('',#5995,#5996,#5068,.T.) ;
#7411 = EDGE_CURVE('',#5996,#5997,#5069,.T.) ;
#7412 = EDGE_CURVE('',#5996,#5998,#5070,.T.) ;
#7413 = EDGE_CURVE('',#5998,#5994,#5071,.T.) ;
#7414 = EDGE_CURVE('',#5999,#6000,#5072,.T.) ;
#7415 = EDGE_CURVE('',#6000,#5999,#5073,.T.) ;
#7416 = EDGE_CURVE('',#6001,#6002,#5074,.T.) ;
#7417 = EDGE_CURVE('',#6002,#6001,#5075,.T.) ;
#7418 = EDGE_CURVE('',#6003,#6004,#5076,.T.) ;
#7419 = EDGE_CURVE('',#6004,#6003,#5077,.T.) ;
#7420 = EDGE_CURVE('',#6005,#6006,#5078,.T.) ;
#7421 = EDGE_CURVE('',#6006,#6007,#5079,.T.) ;
#7422 = EDGE_CURVE('',#6007,#6008,#5080,.T.) ;
#7423 = EDGE_CURVE('',#6009,#6008,#5081,.T.) ;
#7424 = EDGE_CURVE('',#6008,#6005,#5082,.T.) ;
#7425 = EDGE_CURVE('',#6010,#6011,#5083,.T.) ;
#7426 = EDGE_CURVE('',#6011,#6012,#5084,.T.) ;
#7427 = EDGE_CURVE('',#6012,#6013,#5085,.T.) ;
#7428 = EDGE_CURVE('',#6013,#6010,#5086,.T.) ;
#7429 = EDGE_CURVE('',#6014,#6015,#5087,.T.) ;
#7430 = EDGE_CURVE('',#6015,#6016,#5088,.T.) ;
#7431 = EDGE_CURVE('',#6016,#6017,#5089,.T.) ;
#7432 = EDGE_CURVE('',#6017,#6014,#5090,.T.) ;
#7433 = EDGE_CURVE('',#6018,#6019,#5091,.T.) ;
#7434 = EDGE_CURVE('',#6019,#6020,#5092,.T.) ;
#7435 = EDGE_CURVE('',#6020,#6021,#5093,.T.) ;
#7436 = EDGE_CURVE('',#6021,#6018,#5094,.T.) ;
#7437 = EDGE_CURVE('',#6022,#6023,#5095,.T.) ;
#7438 = EDGE_CURVE('',#6023,#6024,#5096,.T.) ;
#7439 = EDGE_CURVE('',#6024,#6025,#5097,.T.) ;
#7440 = EDGE_CURVE('',#6024,#6026,#5098,.T.) ;
#7441 = EDGE_CURVE('',#6026,#6022,#5099,.T.) ;
#7442 = EDGE_CURVE('',#6027,#6028,#5100,.T.) ;
#7443 = EDGE_CURVE('',#6028,#6027,#5101,.T.) ;
#7444 = EDGE_CURVE('',#6029,#6030,#5102,.T.) ;
#7445 = EDGE_CURVE('',#6030,#6029,#5103,.T.) ;
#7446 = EDGE_CURVE('',#6031,#6032,#5104,.T.) ;
#7447 = EDGE_CURVE('',#6032,#6031,#5105,.T.) ;
#7448 = EDGE_CURVE('',#6033,#6034,#5106,.T.) ;
#7449 = EDGE_CURVE('',#6034,#6035,#5107,.T.) ;
#7450 = EDGE_CURVE('',#6035,#6036,#5108,.T.) ;
#7451 = EDGE_CURVE('',#6037,#6036,#5109,.T.) ;
#7452 = EDGE_CURVE('',#6036,#6033,#5110,.T.) ;
#7453 = EDGE_CURVE('',#6038,#6039,#5111,.T.) ;
#7454 = EDGE_CURVE('',#6039,#6040,#5112,.T.) ;
#7455 = EDGE_CURVE('',#6040,#6041,#5113,.T.) ;
#7456 = EDGE_CURVE('',#6041,#6038,#5114,.T.) ;
#7457 = EDGE_CURVE('',#6042,#6043,#5115,.T.) ;
#7458 = EDGE_CURVE('',#6043,#6044,#5116,.T.) ;
#7459 = EDGE_CURVE('',#6044,#6045,#5117,.T.) ;
#7460 = EDGE_CURVE('',#6045,#6042,#5118,.T.) ;
#7461 = EDGE_CURVE('',#6046,#6047,#5119,.T.) ;
#7462 = EDGE_CURVE('',#6047,#6048,#5120,.T.) ;
#7463 = EDGE_CURVE('',#6048,#6049,#5121,.T.) ;
#7464 = EDGE_CURVE('',#6049,#6046,#5122,.T.) ;
#7465 = EDGE_CURVE('',#6050,#6051,#5123,.T.) ;
#7466 = EDGE_CURVE('',#6051,#6052,#5124,.T.) ;
#7467 = EDGE_CURVE('',#6052,#6053,#5125,.T.) ;
#7468 = EDGE_CURVE('',#6052,#6054,#5126,.T.) ;
#7469 = EDGE_CURVE('',#6054,#6050,#5127,.T.) ;
#7470 = EDGE_CURVE('',#6055,#6056,#5128,.T.) ;
#7471 = EDGE_CURVE('',#6056,#6055,#5129,.T.) ;
#7472 = EDGE_CURVE('',#6057,#6058,#5130,.T.) ;
#7473 = EDGE_CURVE('',#6058,#6057,#5131,.T.) ;
#7474 = EDGE_CURVE('',#6059,#6060,#5132,.T.) ;
#7475 = EDGE_CURVE('',#6060,#6059,#5133,.T.) ;
#7476 = EDGE_CURVE('',#6061,#6062,#5134,.T.) ;
#7477 = EDGE_CURVE('',#6062,#6063,#5135,.T.) ;
#7478 = EDGE_CURVE('',#6063,#6064,#5136,.T.) ;
#7479 = EDGE_CURVE('',#6065,#6064,#5137,.T.) ;
#7480 = EDGE_CURVE('',#6064,#6061,#5138,.T.) ;
#7481 = EDGE_CURVE('',#6066,#6067,#5139,.T.) ;
#7482 = EDGE_CURVE('',#6067,#6068,#5140,.T.) ;
#7483 = EDGE_CURVE('',#6068,#6069,#5141,.T.) ;
#7484 = EDGE_CURVE('',#6069,#6066,#5142,.T.) ;
#7485 = EDGE_CURVE('',#6070,#6071,#5143,.T.) ;
#7486 = EDGE_CURVE('',#6071,#6072,#5144,.T.) ;
#7487 = EDGE_CURVE('',#6072,#6073,#5145,.T.) ;
#7488 = EDGE_CURVE('',#6073,#6070,#5146,.T.) ;
#7489 = EDGE_CURVE('',#6074,#6075,#5147,.T.) ;
#7490 = EDGE_CURVE('',#6075,#6076,#5148,.T.) ;
#7491 = EDGE_CURVE('',#6076,#6077,#5149,.T.) ;
#7492 = EDGE_CURVE('',#6077,#6074,#5150,.T.) ;
#7493 = EDGE_CURVE('',#6078,#6079,#5151,.T.) ;
#7494 = EDGE_CURVE('',#6079,#6080,#5152,.T.) ;
#7495 = EDGE_CURVE('',#6080,#6081,#5153,.T.) ;
#7496 = EDGE_CURVE('',#6080,#6082,#5154,.T.) ;
#7497 = EDGE_CURVE('',#6082,#6078,#5155,.T.) ;
#7498 = EDGE_CURVE('',#6083,#6084,#5156,.T.) ;
#7499 = EDGE_CURVE('',#6084,#6083,#5157,.T.) ;
#7500 = EDGE_CURVE('',#6085,#6085,#5158,.T.) ;
#7501 = EDGE_CURVE('',#6085,#6086,#1356,.T.) ;
#7502 = EDGE_CURVE('',#6087,#6086,#277,.T.) ;
#7503 = EDGE_CURVE('',#5976,#6087,#278,.T.) ;
#7504 = EDGE_CURVE('',#6086,#5975,#279,.T.) ;
#7505 = EDGE_CURVE('',#6087,#6088,#1357,.T.) ;
#7506 = EDGE_CURVE('',#5978,#6088,#280,.T.) ;
#7507 = EDGE_CURVE('',#6088,#5977,#281,.T.) ;
#7508 = EDGE_CURVE('',#5979,#5983,#1358,.T.) ;
#7509 = EDGE_CURVE('',#5984,#5982,#282,.T.) ;
#7510 = EDGE_CURVE('',#5985,#5987,#1359,.T.) ;
#7511 = EDGE_CURVE('',#5988,#5986,#283,.T.) ;
#7512 = EDGE_CURVE('',#5989,#5991,#1360,.T.) ;
#7513 = EDGE_CURVE('',#5992,#5990,#284,.T.) ;
#7514 = EDGE_CURVE('',#5993,#5995,#1361,.T.) ;
#7515 = EDGE_CURVE('',#6089,#5994,#285,.T.) ;
#7516 = EDGE_CURVE('',#5998,#6089,#286,.T.) ;
#7517 = EDGE_CURVE('',#6089,#6090,#1362,.T.) ;
#7518 = EDGE_CURVE('',#6091,#6090,#287,.T.) ;
#7519 = EDGE_CURVE('',#6000,#6091,#288,.T.) ;
#7520 = EDGE_CURVE('',#6090,#5999,#289,.T.) ;
#7521 = EDGE_CURVE('',#6091,#6092,#1363,.T.) ;
#7522 = EDGE_CURVE('',#6002,#6092,#290,.T.) ;
#7523 = EDGE_CURVE('',#6092,#6001,#291,.T.) ;
#7524 = EDGE_CURVE('',#6092,#6093,#1364,.T.) ;
#7525 = EDGE_CURVE('',#6094,#6093,#292,.T.) ;
#7526 = EDGE_CURVE('',#6004,#6094,#293,.T.) ;
#7527 = EDGE_CURVE('',#6093,#6003,#294,.T.) ;
#7528 = EDGE_CURVE('',#6094,#6095,#1365,.T.) ;
#7529 = EDGE_CURVE('',#6006,#6095,#295,.T.) ;
#7530 = EDGE_CURVE('',#6095,#6005,#296,.T.) ;
#7531 = EDGE_CURVE('',#6007,#6011,#1366,.T.) ;
#7532 = EDGE_CURVE('',#6012,#6010,#297,.T.) ;
#7533 = EDGE_CURVE('',#6013,#6015,#1367,.T.) ;
#7534 = EDGE_CURVE('',#6016,#6014,#298,.T.) ;
#7535 = EDGE_CURVE('',#6017,#6019,#1368,.T.) ;
#7536 = EDGE_CURVE('',#6020,#6018,#299,.T.) ;
#7537 = EDGE_CURVE('',#6021,#6023,#1369,.T.) ;
#7538 = EDGE_CURVE('',#6096,#6022,#300,.T.) ;
#7539 = EDGE_CURVE('',#6026,#6096,#301,.T.) ;
#7540 = EDGE_CURVE('',#6096,#6097,#1370,.T.) ;
#7541 = EDGE_CURVE('',#6098,#6097,#302,.T.) ;
#7542 = EDGE_CURVE('',#6028,#6098,#303,.T.) ;
#7543 = EDGE_CURVE('',#6097,#6027,#304,.T.) ;
#7544 = EDGE_CURVE('',#6098,#6099,#1371,.T.) ;
#7545 = EDGE_CURVE('',#6030,#6099,#305,.T.) ;
#7546 = EDGE_CURVE('',#6099,#6029,#306,.T.) ;
#7547 = EDGE_CURVE('',#6099,#6100,#1372,.T.) ;
#7548 = EDGE_CURVE('',#6101,#6100,#307,.T.) ;
#7549 = EDGE_CURVE('',#6032,#6101,#308,.T.) ;
#7550 = EDGE_CURVE('',#6100,#6031,#309,.T.) ;
#7551 = EDGE_CURVE('',#6101,#6102,#1373,.T.) ;
#7552 = EDGE_CURVE('',#6034,#6102,#310,.T.) ;
#7553 = EDGE_CURVE('',#6102,#6033,#311,.T.) ;
#7554 = EDGE_CURVE('',#6035,#6039,#1374,.T.) ;
#7555 = EDGE_CURVE('',#6040,#6038,#312,.T.) ;
#7556 = EDGE_CURVE('',#6041,#6043,#1375,.T.) ;
#7557 = EDGE_CURVE('',#6044,#6042,#313,.T.) ;
#7558 = EDGE_CURVE('',#6045,#6047,#1376,.T.) ;
#7559 = EDGE_CURVE('',#6048,#6046,#314,.T.) ;
#7560 = EDGE_CURVE('',#6049,#6051,#1377,.T.) ;
#7561 = EDGE_CURVE('',#6103,#6050,#315,.T.) ;
#7562 = EDGE_CURVE('',#6054,#6103,#316,.T.) ;
#7563 = EDGE_CURVE('',#6103,#6104,#1378,.T.) ;
#7564 = EDGE_CURVE('',#6105,#6104,#317,.T.) ;
#7565 = EDGE_CURVE('',#6056,#6105,#318,.T.) ;
#7566 = EDGE_CURVE('',#6104,#6055,#319,.T.) ;
#7567 = EDGE_CURVE('',#6105,#6106,#1379,.T.) ;
#7568 = EDGE_CURVE('',#6058,#6106,#320,.T.) ;
#7569 = EDGE_CURVE('',#6106,#6057,#321,.T.) ;
#7570 = EDGE_CURVE('',#6106,#6107,#1380,.T.) ;
#7571 = EDGE_CURVE('',#6108,#6107,#322,.T.) ;
#7572 = EDGE_CURVE('',#6060,#6108,#323,.T.) ;
#7573 = EDGE_CURVE('',#6107,#6059,#324,.T.) ;
#7574 = EDGE_CURVE('',#6108,#6109,#1381,.T.) ;
#7575 = EDGE_CURVE('',#6062,#6109,#325,.T.) ;
#7576 = EDGE_CURVE('',#6109,#6061,#326,.T.) ;
#7577 = EDGE_CURVE('',#6063,#6067,#1382,.T.) ;
#7578 = EDGE_CURVE('',#6068,#6066,#327,.T.) ;
#7579 = EDGE_CURVE('',#6069,#6071,#1383,.T.) ;
#7580 = EDGE_CURVE('',#6072,#6070,#328,.T.) ;
#7581 = EDGE_CURVE('',#6073,#6075,#1384,.T.) ;
#7582 = EDGE_CURVE('',#6076,#6074,#329,.T.) ;
#7583 = EDGE_CURVE('',#6077,#6079,#1385,.T.) ;
#7584 = EDGE_CURVE('',#6110,#6078,#330,.T.) ;
#7585 = EDGE_CURVE('',#6082,#6110,#331,.T.) ;
#7586 = EDGE_CURVE('',#6110,#6111,#1386,.T.) ;
#7587 = EDGE_CURVE('',#6112,#6111,#332,.T.) ;
#7588 = EDGE_CURVE('',#6084,#6112,#333,.T.) ;
#7589 = EDGE_CURVE('',#6111,#6083,#334,.T.) ;
#7590 = EDGE_CURVE('',#6112,#6113,#1387,.T.) ;
#7591 = EDGE_CURVE('',#6113,#6113,#5159,.T.) ;
#7592 = EDGE_CURVE('',#6114,#6114,#5160,.T.) ;
#7593 = EDGE_CURVE('',#6114,#6115,#5161,.T.) ;
#7594 = EDGE_CURVE('',#6116,#6114,#5162,.T.) ;
#7595 = EDGE_CURVE('',#6117,#6117,#5163,.T.) ;
#7596 = EDGE_CURVE('',#6118,#6117,#5164,.T.) ;
#7597 = EDGE_CURVE('',#6117,#6119,#5165,.T.) ;
#7598 = EDGE_CURVE('',#6120,#6121,#5166,.T.) ;
#7599 = EDGE_CURVE('',#6121,#6120,#956,.T.) ;
#7600 = EDGE_CURVE('',#6120,#6121,#5167,.T.) ;
#7601 = EDGE_CURVE('',#6122,#6122,#5168,.T.) ;
#7602 = EDGE_CURVE('',#6123,#6122,#5169,.T.) ;
#7603 = EDGE_CURVE('',#6122,#6124,#5170,.T.) ;
#7604 = EDGE_CURVE('',#6125,#6124,#957,.T.) ;
#7605 = EDGE_CURVE('',#6124,#6125,#5171,.T.) ;
#7606 = EDGE_CURVE('',#6125,#6124,#5172,.T.) ;
#7607 = EDGE_CURVE('',#6126,#6126,#5173,.T.) ;
#7608 = EDGE_CURVE('',#6126,#6127,#5174,.T.) ;
#7609 = EDGE_CURVE('',#6127,#6127,#5175,.T.) ;
#7610 = EDGE_CURVE('',#6127,#6128,#5176,.T.) ;
#7611 = EDGE_CURVE('',#6129,#6126,#5177,.T.) ;
#7612 = EDGE_CURVE('',#6130,#6130,#5178,.T.) ;
#7613 = EDGE_CURVE('',#6131,#6130,#5179,.T.) ;
#7614 = EDGE_CURVE('',#6130,#6132,#5180,.T.) ;
#7615 = EDGE_CURVE('',#6133,#6133,#5181,.T.) ;
#7616 = EDGE_CURVE('',#6134,#6133,#5182,.T.) ;
#7617 = EDGE_CURVE('',#6133,#6135,#5183,.T.) ;
#7618 = EDGE_CURVE('',#6135,#6135,#5184,.T.) ;
#7619 = EDGE_CURVE('',#6135,#6136,#5185,.T.) ;
#7620 = EDGE_CURVE('',#6137,#6137,#5186,.T.) ;
#7621 = EDGE_CURVE('',#6137,#6138,#5187,.T.) ;
#7622 = EDGE_CURVE('',#6138,#6138,#5188,.T.) ;
#7623 = EDGE_CURVE('',#6138,#6139,#5189,.T.) ;
#7624 = EDGE_CURVE('',#6140,#6137,#5190,.T.) ;
#7625 = EDGE_CURVE('',#6141,#6141,#5191,.T.) ;
#7626 = EDGE_CURVE('',#6142,#6141,#5192,.T.) ;
#7627 = EDGE_CURVE('',#6141,#6143,#5193,.T.) ;
#7628 = EDGE_CURVE('',#6144,#6144,#5194,.T.) ;
#7629 = EDGE_CURVE('',#6145,#6144,#5195,.T.) ;
#7630 = EDGE_CURVE('',#6144,#6146,#5196,.T.) ;
#7631 = EDGE_CURVE('',#6146,#6146,#5197,.T.) ;
#7632 = EDGE_CURVE('',#6146,#6147,#5198,.T.) ;
#7633 = EDGE_CURVE('',#6148,#6148,#5199,.T.) ;
#7634 = EDGE_CURVE('',#6148,#6149,#5200,.T.) ;
#7635 = EDGE_CURVE('',#6149,#6149,#5201,.T.) ;
#7636 = EDGE_CURVE('',#6149,#6150,#5202,.T.) ;
#7637 = EDGE_CURVE('',#6151,#6148,#5203,.T.) ;
#7638 = EDGE_CURVE('',#6152,#6152,#5204,.T.) ;
#7639 = EDGE_CURVE('',#6153,#6152,#5205,.T.) ;
#7640 = EDGE_CURVE('',#6152,#6154,#5206,.T.) ;
#7641 = EDGE_CURVE('',#6155,#6155,#5207,.T.) ;
#7642 = EDGE_CURVE('',#6156,#6155,#5208,.T.) ;
#7643 = EDGE_CURVE('',#6155,#6157,#5209,.T.) ;
#7644 = EDGE_CURVE('',#6157,#6157,#5210,.T.) ;
#7645 = EDGE_CURVE('',#6157,#6158,#5211,.T.) ;
#7646 = EDGE_CURVE('',#6159,#6159,#5212,.T.) ;
#7647 = EDGE_CURVE('',#6159,#6160,#5213,.T.) ;
#7648 = EDGE_CURVE('',#6160,#6160,#5214,.T.) ;
#7649 = EDGE_CURVE('',#6160,#6161,#5215,.T.) ;
#7650 = EDGE_CURVE('',#6162,#6162,#5216,.T.) ;
#7651 = EDGE_CURVE('',#6163,#6163,#5217,.T.) ;
#7652 = EDGE_CURVE('',#6163,#6164,#5218,.T.) ;
#7653 = EDGE_CURVE('',#6164,#6164,#5219,.T.) ;
#7654 = EDGE_CURVE('',#6165,#6165,#5220,.T.) ;
#7655 = EDGE_CURVE('',#6166,#6165,#5221,.T.) ;
#7656 = EDGE_CURVE('',#6167,#6167,#5222,.T.) ;
#7657 = EDGE_CURVE('',#6168,#6168,#5223,.T.) ;
#7658 = EDGE_CURVE('',#6169,#6169,#5224,.T.) ;
#7659 = EDGE_CURVE('',#6170,#6171,#5225,.T.) ;
#7660 = EDGE_CURVE('',#6172,#6170,#5226,.T.) ;
#7661 = EDGE_CURVE('',#6171,#6170,#5227,.T.) ;
#7662 = EDGE_CURVE('',#6171,#6173,#5228,.T.) ;
#7663 = EDGE_CURVE('',#6174,#6175,#5229,.T.) ;
#7664 = EDGE_CURVE('',#6176,#6174,#5230,.T.) ;
#7665 = EDGE_CURVE('',#6175,#6174,#5231,.T.) ;
#7666 = EDGE_CURVE('',#6175,#6177,#5232,.T.) ;
#7667 = EDGE_CURVE('',#6178,#6178,#5233,.T.) ;
#7668 = EDGE_CURVE('',#6179,#6179,#5234,.T.) ;
#7669 = EDGE_CURVE('',#6180,#6181,#5235,.T.) ;
#7670 = EDGE_CURVE('',#6181,#6180,#5236,.T.) ;
#7671 = EDGE_CURVE('',#6180,#6181,#958,.T.) ;
#7672 = EDGE_CURVE('',#6182,#6182,#5237,.T.) ;
#7673 = EDGE_CURVE('',#6183,#6184,#5238,.T.) ;
#7674 = EDGE_CURVE('',#6184,#6183,#5239,.T.) ;
#7675 = EDGE_CURVE('',#6185,#6183,#5240,.T.) ;
#7676 = EDGE_CURVE('',#6184,#6186,#5241,.T.) ;
#7677 = EDGE_CURVE('',#6187,#6188,#5242,.T.) ;
#7678 = EDGE_CURVE('',#6187,#6188,#5243,.T.) ;
#7679 = EDGE_CURVE('',#6189,#6190,#5244,.T.) ;
#7680 = EDGE_CURVE('',#6191,#6189,#5245,.T.) ;
#7681 = EDGE_CURVE('',#6190,#6189,#5246,.T.) ;
#7682 = EDGE_CURVE('',#6190,#6192,#5247,.T.) ;
#7683 = EDGE_CURVE('',#6187,#6188,#959,.T.) ;
#7684 = EDGE_CURVE('',#6193,#6194,#5248,.T.) ;
#7685 = EDGE_CURVE('',#6194,#6195,#5249,.T.) ;
#7686 = EDGE_CURVE('',#6195,#6196,#5250,.T.) ;
#7687 = EDGE_CURVE('',#6196,#6193,#5251,.T.) ;
#7688 = EDGE_CURVE('',#6197,#6198,#5252,.T.) ;
#7689 = EDGE_CURVE('',#6198,#6199,#5253,.T.) ;
#7690 = EDGE_CURVE('',#6199,#6200,#5254,.T.) ;
#7691 = EDGE_CURVE('',#6200,#6197,#5255,.T.) ;
#7692 = EDGE_CURVE('',#6201,#6202,#5256,.T.) ;
#7693 = EDGE_CURVE('',#6202,#6203,#5257,.T.) ;
#7694 = EDGE_CURVE('',#6203,#6204,#5258,.T.) ;
#7695 = EDGE_CURVE('',#6204,#6201,#5259,.T.) ;
#7696 = EDGE_CURVE('',#6205,#6206,#5260,.T.) ;
#7697 = EDGE_CURVE('',#6206,#6207,#5261,.T.) ;
#7698 = EDGE_CURVE('',#6207,#6208,#5262,.T.) ;
#7699 = EDGE_CURVE('',#6208,#6205,#5263,.T.) ;
#7700 = EDGE_CURVE('',#6209,#6210,#5264,.T.) ;
#7701 = EDGE_CURVE('',#6210,#6211,#5265,.T.) ;
#7702 = EDGE_CURVE('',#6211,#6212,#5266,.T.) ;
#7703 = EDGE_CURVE('',#6212,#6209,#5267,.T.) ;
#7704 = EDGE_CURVE('',#6213,#6214,#5268,.T.) ;
#7705 = EDGE_CURVE('',#6214,#6215,#5269,.T.) ;
#7706 = EDGE_CURVE('',#6215,#6216,#5270,.T.) ;
#7707 = EDGE_CURVE('',#6216,#6213,#5271,.T.) ;
#7708 = EDGE_CURVE('',#6217,#6218,#5272,.T.) ;
#7709 = EDGE_CURVE('',#6217,#6218,#5273,.T.) ;
#7710 = EDGE_CURVE('',#6219,#6220,#5274,.T.) ;
#7711 = EDGE_CURVE('',#6221,#6220,#5275,.T.) ;
#7712 = EDGE_CURVE('',#6220,#6222,#5276,.T.) ;
#7713 = EDGE_CURVE('',#6222,#6219,#5277,.T.) ;
#7714 = EDGE_CURVE('',#6223,#6223,#5278,.T.) ;
#7715 = EDGE_CURVE('',#6223,#6224,#1388,.T.) ;
#7716 = EDGE_CURVE('',#6224,#6217,#960,.T.) ;
#7717 = EDGE_CURVE('',#6218,#6224,#961,.T.) ;
#7718 = EDGE_CURVE('',#6225,#6225,#5279,.T.) ;
#7719 = EDGE_CURVE('',#6225,#6226,#1389,.T.) ;
#7720 = EDGE_CURVE('',#6227,#6226,#335,.T.) ;
#7721 = EDGE_CURVE('',#6228,#6227,#5280,.T.) ;
#7722 = EDGE_CURVE('',#6229,#6228,#5281,.T.) ;
#7723 = EDGE_CURVE('',#6226,#6229,#336,.T.) ;
#7724 = EDGE_CURVE('',#6230,#6230,#5282,.T.) ;
#7725 = EDGE_CURVE('',#6229,#6231,#1390,.T.) ;
#7726 = EDGE_CURVE('',#6232,#6231,#337,.T.) ;
#7727 = EDGE_CURVE('',#6233,#6232,#5283,.T.) ;
#7728 = EDGE_CURVE('',#6231,#6233,#338,.T.) ;
#7729 = EDGE_CURVE('',#6227,#6229,#5284,.T.) ;
#7730 = EDGE_CURVE('',#6234,#6235,#962,.T.) ;
#7731 = EDGE_CURVE('',#6235,#6236,#963,.T.) ;
#7732 = EDGE_CURVE('',#6234,#6236,#5285,.T.) ;
#7733 = EDGE_CURVE('',#6237,#6233,#5286,.T.) ;
#7734 = EDGE_CURVE('',#6237,#6194,#1391,.T.) ;
#7735 = EDGE_CURVE('',#6195,#6193,#339,.T.) ;
#7736 = EDGE_CURVE('',#6232,#6237,#5287,.T.) ;
#7737 = EDGE_CURVE('',#6196,#6198,#1392,.T.) ;
#7738 = EDGE_CURVE('',#6199,#6197,#340,.T.) ;
#7739 = EDGE_CURVE('',#6200,#6238,#1393,.T.) ;
#7740 = EDGE_CURVE('',#6239,#6238,#5288,.T.) ;
#7741 = EDGE_CURVE('',#6240,#6239,#341,.T.) ;
#7742 = EDGE_CURVE('',#6238,#6240,#5289,.T.) ;
#7743 = EDGE_CURVE('',#6241,#6239,#5290,.T.) ;
#7744 = EDGE_CURVE('',#6241,#6242,#1394,.T.) ;
#7745 = EDGE_CURVE('',#6243,#6242,#5291,.T.) ;
#7746 = EDGE_CURVE('',#6244,#6243,#342,.T.) ;
#7747 = EDGE_CURVE('',#6242,#6244,#5292,.T.) ;
#7748 = EDGE_CURVE('',#6240,#6241,#5293,.T.) ;
#7749 = EDGE_CURVE('',#6245,#6243,#5294,.T.) ;
#7750 = EDGE_CURVE('',#6245,#6202,#1395,.T.) ;
#7751 = EDGE_CURVE('',#6203,#6201,#343,.T.) ;
#7752 = EDGE_CURVE('',#6244,#6245,#5295,.T.) ;
#7753 = EDGE_CURVE('',#6204,#6206,#1396,.T.) ;
#7754 = EDGE_CURVE('',#6207,#6205,#344,.T.) ;
#7755 = EDGE_CURVE('',#6208,#6246,#1397,.T.) ;
#7756 = EDGE_CURVE('',#6247,#6246,#5296,.T.) ;
#7757 = EDGE_CURVE('',#6248,#6247,#345,.T.) ;
#7758 = EDGE_CURVE('',#6246,#6248,#5297,.T.) ;
#7759 = EDGE_CURVE('',#6249,#6247,#5298,.T.) ;
#7760 = EDGE_CURVE('',#6249,#6250,#1398,.T.) ;
#7761 = EDGE_CURVE('',#6251,#6250,#5299,.T.) ;
#7762 = EDGE_CURVE('',#6252,#6251,#346,.T.) ;
#7763 = EDGE_CURVE('',#6250,#6252,#5300,.T.) ;
#7764 = EDGE_CURVE('',#6248,#6249,#5301,.T.) ;
#7765 = EDGE_CURVE('',#6253,#6251,#5302,.T.) ;
#7766 = EDGE_CURVE('',#6253,#6210,#1399,.T.) ;
#7767 = EDGE_CURVE('',#6211,#6209,#347,.T.) ;
#7768 = EDGE_CURVE('',#6252,#6253,#5303,.T.) ;
#7769 = EDGE_CURVE('',#6212,#6214,#1400,.T.) ;
#7770 = EDGE_CURVE('',#6215,#6213,#348,.T.) ;
#7771 = EDGE_CURVE('',#6216,#6254,#1401,.T.) ;
#7772 = EDGE_CURVE('',#6255,#6254,#5304,.T.) ;
#7773 = EDGE_CURVE('',#6256,#6255,#349,.T.) ;
#7774 = EDGE_CURVE('',#6254,#6256,#5305,.T.) ;
#7775 = EDGE_CURVE('',#6257,#6255,#5306,.T.) ;
#7776 = EDGE_CURVE('',#6257,#6258,#1402,.T.) ;
#7777 = EDGE_CURVE('',#6259,#6258,#5307,.T.) ;
#7778 = EDGE_CURVE('',#6260,#6259,#350,.T.) ;
#7779 = EDGE_CURVE('',#6258,#6260,#5308,.T.) ;
#7780 = EDGE_CURVE('',#6256,#6257,#5309,.T.) ;
#7781 = EDGE_CURVE('',#6261,#6259,#5310,.T.) ;
#7782 = EDGE_CURVE('',#6261,#6222,#1403,.T.) ;
#7783 = EDGE_CURVE('',#6262,#6219,#351,.T.) ;
#7784 = EDGE_CURVE('',#6222,#6262,#352,.T.) ;
#7785 = EDGE_CURVE('',#6260,#6261,#5311,.T.) ;
#7786 = EDGE_CURVE('',#6262,#6263,#1404,.T.) ;
#7787 = EDGE_CURVE('',#6263,#6263,#5312,.T.) ;
#7788 = EDGE_CURVE('',#6237,#6264,#5313,.T.) ;
#7789 = EDGE_CURVE('',#6234,#6236,#5314,.T.) ;
#7790 = EDGE_CURVE('',#6235,#6230,#1405,.T.) ;
#7791 = EDGE_CURVE('',#6265,#6228,#5315,.T.) ;
#7792 = EDGE_CURVE('',#6266,#6266,#5316,.T.) ;
#7793 = EDGE_CURVE('',#6267,#6267,#5317,.T.) ;
#7794 = EDGE_CURVE('',#6268,#6268,#5318,.T.) ;
#7795 = EDGE_CURVE('',#6268,#6269,#5319,.T.) ;
#7796 = EDGE_CURVE('',#6270,#6268,#5320,.T.) ;
#7797 = EDGE_CURVE('',#6271,#6271,#5321,.T.) ;
#7798 = EDGE_CURVE('',#6271,#6272,#5322,.T.) ;
#7799 = EDGE_CURVE('',#6273,#6271,#5323,.T.) ;
#7800 = EDGE_CURVE('',#6274,#6274,#5324,.T.) ;
#7801 = EDGE_CURVE('',#6274,#6275,#5325,.T.) ;
#7802 = EDGE_CURVE('',#6276,#6274,#5326,.T.) ;
#7803 = EDGE_CURVE('',#6277,#6277,#5327,.T.) ;
#7804 = EDGE_CURVE('',#6277,#6278,#5328,.T.) ;
#7805 = EDGE_CURVE('',#6279,#6277,#5329,.T.) ;
#7806 = EDGE_CURVE('',#6280,#6281,#5330,.T.) ;
#7807 = EDGE_CURVE('',#6282,#6280,#1406,.T.) ;
#7808 = EDGE_CURVE('',#6283,#6282,#5331,.T.) ;
#7809 = EDGE_CURVE('',#6283,#6281,#1407,.T.) ;
#7810 = EDGE_CURVE('',#6281,#6284,#1408,.T.) ;
#7811 = EDGE_CURVE('',#6285,#6283,#1409,.T.) ;
#7812 = EDGE_CURVE('',#6285,#6284,#1410,.T.) ;
#7813 = EDGE_CURVE('',#6284,#6286,#5332,.T.) ;
#7814 = EDGE_CURVE('',#6287,#6285,#5333,.T.) ;
#7815 = EDGE_CURVE('',#6287,#6286,#1411,.T.) ;
#7816 = EDGE_CURVE('',#6286,#6280,#1412,.T.) ;
#7817 = EDGE_CURVE('',#6282,#6287,#1413,.T.) ;
#7818 = EDGE_CURVE('',#6288,#6288,#5334,.T.) ;
#7819 = EDGE_CURVE('',#6288,#6289,#1414,.T.) ;
#7820 = EDGE_CURVE('',#6289,#6289,#5335,.T.) ;
#7821 = EDGE_CURVE('',#6290,#6291,#5336,.T.) ;
#7822 = EDGE_CURVE('',#6292,#6290,#1415,.T.) ;
#7823 = EDGE_CURVE('',#6293,#6292,#5337,.T.) ;
#7824 = EDGE_CURVE('',#6293,#6291,#1416,.T.) ;
#7825 = EDGE_CURVE('',#6291,#6294,#1417,.T.) ;
#7826 = EDGE_CURVE('',#6295,#6293,#1418,.T.) ;
#7827 = EDGE_CURVE('',#6295,#6294,#1419,.T.) ;
#7828 = EDGE_CURVE('',#6294,#6296,#5338,.T.) ;
#7829 = EDGE_CURVE('',#6297,#6295,#5339,.T.) ;
#7830 = EDGE_CURVE('',#6297,#6296,#1420,.T.) ;
#7831 = EDGE_CURVE('',#6296,#6290,#1421,.T.) ;
#7832 = EDGE_CURVE('',#6292,#6297,#1422,.T.) ;
#7833 = EDGE_CURVE('',#6298,#6298,#5340,.T.) ;
#7834 = EDGE_CURVE('',#6298,#6299,#1423,.T.) ;
#7835 = EDGE_CURVE('',#6299,#6299,#5341,.T.) ;
#7836 = EDGE_CURVE('',#6300,#6301,#1424,.T.) ;
#7837 = EDGE_CURVE('',#6300,#6302,#1425,.T.) ;
#7838 = EDGE_CURVE('',#6302,#6303,#1426,.T.) ;
#7839 = EDGE_CURVE('',#6303,#6301,#1427,.T.) ;
#7840 = EDGE_CURVE('',#6304,#6303,#1428,.T.) ;
#7841 = EDGE_CURVE('',#6305,#6302,#1429,.T.) ;
#7842 = EDGE_CURVE('',#6304,#6305,#1430,.T.) ;
#7843 = EDGE_CURVE('',#6301,#6306,#1431,.T.) ;
#7844 = EDGE_CURVE('',#6307,#6306,#1432,.T.) ;
#7845 = EDGE_CURVE('',#6300,#6307,#1433,.T.) ;
#7846 = EDGE_CURVE('',#6308,#6309,#1434,.T.) ;
#7847 = EDGE_CURVE('',#6306,#6309,#1435,.T.) ;
#7848 = EDGE_CURVE('',#6308,#6304,#1436,.T.) ;
#7849 = EDGE_CURVE('',#6305,#6310,#1437,.T.) ;
#7850 = EDGE_CURVE('',#6310,#6308,#1438,.T.) ;
#7851 = EDGE_CURVE('',#6309,#6311,#1439,.T.) ;
#7852 = EDGE_CURVE('',#6311,#6307,#1440,.T.) ;
#7853 = EDGE_CURVE('',#6310,#6311,#1441,.T.) ;
#7854 = EDGE_CURVE('',#6312,#6313,#964,.T.) ;
#7855 = EDGE_CURVE('',#6312,#6314,#965,.F.) ;
#7856 = EDGE_CURVE('',#6314,#6315,#966,.F.) ;
#7857 = EDGE_CURVE('',#6316,#6315,#967,.T.) ;
#7858 = EDGE_CURVE('',#6317,#6316,#968,.T.) ;
#7859 = EDGE_CURVE('',#6313,#6317,#969,.T.) ;
#7860 = EDGE_CURVE('',#6318,#6312,#970,.T.) ;
#7861 = EDGE_CURVE('',#6318,#6319,#971,.F.) ;
#7862 = EDGE_CURVE('',#6319,#6320,#972,.F.) ;
#7863 = EDGE_CURVE('',#6315,#6320,#973,.T.) ;
#7864 = EDGE_CURVE('',#6321,#6318,#974,.T.) ;
#7865 = EDGE_CURVE('',#6321,#6322,#975,.F.) ;
#7866 = EDGE_CURVE('',#6322,#6323,#976,.F.) ;
#7867 = EDGE_CURVE('',#6320,#6323,#977,.T.) ;
#7868 = EDGE_CURVE('',#6313,#6321,#978,.T.) ;
#7869 = EDGE_CURVE('',#6323,#6316,#979,.T.) ;
#7870 = EDGE_CURVE('',#6324,#6325,#5342,.T.) ;
#7871 = EDGE_CURVE('',#6326,#6324,#5343,.T.) ;
#7872 = EDGE_CURVE('',#6327,#6326,#5344,.T.) ;
#7873 = EDGE_CURVE('',#6325,#6327,#5345,.T.) ;
#7874 = EDGE_CURVE('',#6328,#6329,#1442,.T.) ;
#7875 = EDGE_CURVE('',#6329,#6330,#1443,.T.) ;
#7876 = EDGE_CURVE('',#6330,#6331,#1444,.T.) ;
#7877 = EDGE_CURVE('',#6331,#6328,#1445,.T.) ;
#7878 = EDGE_CURVE('',#6328,#6324,#1446,.T.) ;
#7879 = EDGE_CURVE('',#6329,#6325,#1447,.T.) ;
#7880 = EDGE_CURVE('',#6330,#6327,#1448,.T.) ;
#7881 = EDGE_CURVE('',#6331,#6326,#1449,.T.) ;
#7882 = EDGE_CURVE('',#6332,#6332,#5346,.T.) ;
#7883 = EDGE_CURVE('',#6332,#6333,#1450,.T.) ;
#7884 = EDGE_CURVE('',#6333,#6333,#5347,.T.) ;
#7885 = EDGE_CURVE('',#6334,#6335,#1451,.T.) ;
#7886 = EDGE_CURVE('',#6336,#6334,#1452,.T.) ;
#7887 = EDGE_CURVE('',#6336,#6337,#1453,.T.) ;
#7888 = EDGE_CURVE('',#6337,#6335,#1454,.T.) ;
#7889 = EDGE_CURVE('',#6335,#6338,#1455,.T.) ;
#7890 = EDGE_CURVE('',#6337,#6339,#1456,.T.) ;
#7891 = EDGE_CURVE('',#6339,#6338,#1457,.T.) ;
#7892 = EDGE_CURVE('',#6340,#6336,#1458,.T.) ;
#7893 = EDGE_CURVE('',#6339,#6340,#1459,.T.) ;
#7894 = EDGE_CURVE('',#6338,#6341,#1460,.T.) ;
#7895 = EDGE_CURVE('',#6340,#6341,#1461,.T.) ;
#7896 = EDGE_CURVE('',#6341,#6334,#1462,.T.) ;
#7897 = EDGE_CURVE('',#6342,#6343,#1463,.T.) ;
#7898 = EDGE_CURVE('',#6343,#6344,#1464,.T.) ;
#7899 = EDGE_CURVE('',#6344,#6345,#1465,.T.) ;
#7900 = EDGE_CURVE('',#6345,#6342,#1466,.T.) ;
#7901 = EDGE_CURVE('',#6346,#6344,#1467,.T.) ;
#7902 = EDGE_CURVE('',#6347,#6343,#1468,.T.) ;
#7903 = EDGE_CURVE('',#6346,#6347,#1469,.T.) ;
#7904 = EDGE_CURVE('',#6348,#6345,#1470,.T.) ;
#7905 = EDGE_CURVE('',#6348,#6346,#1471,.T.) ;
#7906 = EDGE_CURVE('',#6349,#6342,#1472,.T.) ;
#7907 = EDGE_CURVE('',#6349,#6348,#1473,.T.) ;
#7908 = EDGE_CURVE('',#6347,#6349,#1474,.T.) ;
#7909 = EDGE_CURVE('',#6350,#6351,#1475,.T.) ;
#7910 = EDGE_CURVE('',#6351,#6352,#1476,.T.) ;
#7911 = EDGE_CURVE('',#6352,#6353,#1477,.T.) ;
#7912 = EDGE_CURVE('',#6353,#6350,#1478,.T.) ;
#7913 = EDGE_CURVE('',#6354,#6355,#1479,.T.) ;
#7914 = EDGE_CURVE('',#6355,#6356,#1480,.T.) ;
#7915 = EDGE_CURVE('',#6356,#6357,#1481,.T.) ;
#7916 = EDGE_CURVE('',#6357,#6354,#1482,.T.) ;
#7917 = EDGE_CURVE('',#6353,#6356,#1483,.T.) ;
#7918 = EDGE_CURVE('',#6350,#6355,#1484,.T.) ;
#7919 = EDGE_CURVE('',#6352,#6357,#1485,.T.) ;
#7920 = EDGE_CURVE('',#6351,#6354,#1486,.T.) ;
#7921 = EDGE_CURVE('',#6358,#6359,#1487,.T.) ;
#7922 = EDGE_CURVE('',#6358,#6360,#1488,.T.) ;
#7923 = EDGE_CURVE('',#6360,#6361,#1489,.T.) ;
#7924 = EDGE_CURVE('',#6361,#6362,#1490,.T.) ;
#7925 = EDGE_CURVE('',#6363,#6362,#1491,.T.) ;
#7926 = EDGE_CURVE('',#6363,#6364,#1492,.T.) ;
#7927 = EDGE_CURVE('',#6365,#6364,#1493,.T.) ;
#7928 = EDGE_CURVE('',#6359,#6365,#1494,.T.) ;
#7929 = EDGE_CURVE('',#6366,#6367,#1495,.T.) ;
#7930 = EDGE_CURVE('',#6368,#6366,#1496,.T.) ;
#7931 = EDGE_CURVE('',#6369,#6368,#1497,.T.) ;
#7932 = EDGE_CURVE('',#6367,#6369,#1498,.T.) ;
#7933 = EDGE_CURVE('',#6370,#6366,#5348,.T.) ;
#7934 = EDGE_CURVE('',#6371,#6370,#1499,.T.) ;
#7935 = EDGE_CURVE('',#6372,#6371,#1500,.T.) ;
#7936 = EDGE_CURVE('',#6372,#6373,#1501,.T.) ;
#7937 = EDGE_CURVE('',#6373,#6368,#1502,.T.) ;
#7938 = EDGE_CURVE('',#6367,#6374,#5349,.T.) ;
#7939 = EDGE_CURVE('',#6375,#6369,#1503,.T.) ;
#7940 = EDGE_CURVE('',#6375,#6376,#1504,.T.) ;
#7941 = EDGE_CURVE('',#6377,#6376,#1505,.T.) ;
#7942 = EDGE_CURVE('',#6374,#6377,#1506,.T.) ;
#7943 = EDGE_CURVE('',#6378,#6379,#1507,.T.) ;
#7944 = EDGE_CURVE('',#6378,#6363,#1508,.T.) ;
#7945 = EDGE_CURVE('',#6362,#6380,#1509,.T.) ;
#7946 = EDGE_CURVE('',#6381,#6380,#5350,.T.) ;
#7947 = EDGE_CURVE('',#6379,#6381,#1510,.T.) ;
#7948 = EDGE_CURVE('',#6376,#6382,#5351,.T.) ;
#7949 = EDGE_CURVE('',#6382,#6375,#1511,.T.) ;
#7950 = EDGE_CURVE('',#6364,#6378,#5352,.T.) ;
#7951 = EDGE_CURVE('',#6383,#6372,#5353,.T.) ;
#7952 = EDGE_CURVE('',#6373,#6383,#1512,.T.) ;
#7953 = EDGE_CURVE('',#6384,#6358,#5354,.T.) ;
#7954 = EDGE_CURVE('',#6360,#6384,#1513,.T.) ;
#7955 = EDGE_CURVE('',#6380,#6385,#1514,.T.) ;
#7956 = EDGE_CURVE('',#6385,#6361,#1515,.T.) ;
#7957 = EDGE_CURVE('',#6386,#6384,#1516,.T.) ;
#7958 = EDGE_CURVE('',#6387,#6386,#1517,.T.) ;
#7959 = EDGE_CURVE('',#6385,#6387,#5355,.T.) ;
#7960 = EDGE_CURVE('',#6388,#6383,#1518,.T.) ;
#7961 = EDGE_CURVE('',#6389,#6388,#1519,.T.) ;
#7962 = EDGE_CURVE('',#6382,#6389,#1520,.T.) ;
#7963 = EDGE_CURVE('',#6381,#6390,#1521,.T.) ;
#7964 = EDGE_CURVE('',#6379,#6390,#5356,.T.) ;
#7965 = EDGE_CURVE('',#6391,#6386,#5357,.T.) ;
#7966 = EDGE_CURVE('',#6391,#6387,#1522,.T.) ;
#7967 = EDGE_CURVE('',#6392,#6365,#5358,.T.) ;
#7968 = EDGE_CURVE('',#6359,#6392,#5359,.T.) ;
#7969 = EDGE_CURVE('',#6393,#6377,#5360,.T.) ;
#7970 = EDGE_CURVE('',#6393,#6374,#1523,.T.) ;
#7971 = EDGE_CURVE('',#6389,#6388,#5361,.T.) ;
#7972 = EDGE_CURVE('',#6394,#6394,#5362,.T.) ;
#7973 = EDGE_CURVE('',#6394,#6395,#1524,.T.) ;
#7974 = EDGE_CURVE('',#6396,#6395,#980,.T.) ;
#7975 = EDGE_CURVE('',#6395,#6396,#981,.T.) ;
#7976 = EDGE_CURVE('',#6397,#6397,#5363,.T.) ;
#7977 = EDGE_CURVE('',#6397,#6398,#1525,.T.) ;
#7978 = EDGE_CURVE('',#6398,#6398,#5364,.T.) ;
#7979 = EDGE_CURVE('',#6399,#6399,#5365,.T.) ;
#7980 = EDGE_CURVE('',#6399,#6400,#1526,.T.) ;
#7981 = EDGE_CURVE('',#6400,#6400,#5366,.T.) ;
#7982 = EDGE_CURVE('',#6401,#6401,#5367,.T.) ;
#7983 = EDGE_CURVE('',#6401,#6402,#1527,.T.) ;
#7984 = EDGE_CURVE('',#6402,#6402,#5368,.T.) ;
#7985 = EDGE_CURVE('',#6403,#6391,#982,.T.) ;
#7986 = EDGE_CURVE('',#6370,#6403,#1528,.T.) ;
#7987 = EDGE_CURVE('',#6390,#6393,#983,.T.) ;
#7988 = EDGE_CURVE('',#6371,#6403,#5369,.T.) ;
#7989 = EDGE_CURVE('',#6392,#6404,#1529,.T.) ;
#7990 = EDGE_CURVE('',#6404,#6404,#5370,.T.) ;
#7991 = EDGE_CURVE('',#6405,#6406,#1530,.T.) ;
#7992 = EDGE_CURVE('',#6406,#6407,#1531,.T.) ;
#7993 = EDGE_CURVE('',#6407,#6408,#1532,.T.) ;
#7994 = EDGE_CURVE('',#6408,#6405,#1533,.T.) ;
#7995 = EDGE_CURVE('',#6409,#6410,#1534,.T.) ;
#7996 = EDGE_CURVE('',#6410,#6411,#1535,.T.) ;
#7997 = EDGE_CURVE('',#6411,#6412,#1536,.T.) ;
#7998 = EDGE_CURVE('',#6412,#6409,#1537,.T.) ;
#7999 = EDGE_CURVE('',#6408,#6411,#1538,.T.) ;
#8000 = EDGE_CURVE('',#6405,#6410,#1539,.T.) ;
#8001 = EDGE_CURVE('',#6407,#6412,#1540,.T.) ;
#8002 = EDGE_CURVE('',#6406,#6409,#1541,.T.) ;
#8003 = EDGE_CURVE('',#6413,#6413,#5371,.T.) ;
#8004 = EDGE_CURVE('',#6413,#6414,#1542,.T.) ;
#8005 = EDGE_CURVE('',#6414,#6414,#5372,.T.) ;
#8006 = EDGE_CURVE('',#6415,#6416,#5373,.T.) ;
#8007 = EDGE_CURVE('',#6417,#6415,#1543,.T.) ;
#8008 = EDGE_CURVE('',#6418,#6417,#5374,.T.) ;
#8009 = EDGE_CURVE('',#6416,#6418,#1544,.T.) ;
#8010 = EDGE_CURVE('',#6417,#6419,#5375,.T.) ;
#8011 = EDGE_CURVE('',#6419,#6420,#5376,.T.) ;
#8012 = EDGE_CURVE('',#6420,#6421,#5377,.T.) ;
#8013 = EDGE_CURVE('',#6421,#6422,#5378,.T.) ;
#8014 = EDGE_CURVE('',#6422,#6423,#5379,.T.) ;
#8015 = EDGE_CURVE('',#6423,#6424,#5380,.T.) ;
#8016 = EDGE_CURVE('',#6424,#6425,#5381,.T.) ;
#8017 = EDGE_CURVE('',#6425,#6426,#5382,.T.) ;
#8018 = EDGE_CURVE('',#6426,#6427,#5383,.T.) ;
#8019 = EDGE_CURVE('',#6427,#6428,#5384,.T.) ;
#8020 = EDGE_CURVE('',#6428,#6429,#5385,.T.) ;
#8021 = EDGE_CURVE('',#6429,#6430,#5386,.T.) ;
#8022 = EDGE_CURVE('',#6430,#6431,#5387,.T.) ;
#8023 = EDGE_CURVE('',#6431,#6432,#5388,.T.) ;
#8024 = EDGE_CURVE('',#6432,#6418,#5389,.T.) ;
#8025 = EDGE_CURVE('',#6433,#6415,#5390,.T.) ;
#8026 = EDGE_CURVE('',#6433,#6419,#1545,.T.) ;
#8027 = EDGE_CURVE('',#6434,#6433,#5391,.T.) ;
#8028 = EDGE_CURVE('',#6420,#6434,#1546,.T.) ;
#8029 = EDGE_CURVE('',#6435,#6434,#5392,.T.) ;
#8030 = EDGE_CURVE('',#6435,#6421,#1547,.T.) ;
#8031 = EDGE_CURVE('',#6436,#6435,#5393,.T.) ;
#8032 = EDGE_CURVE('',#6422,#6436,#1548,.T.) ;
#8033 = EDGE_CURVE('',#6437,#6436,#5394,.T.) ;
#8034 = EDGE_CURVE('',#6437,#6423,#1549,.T.) ;
#8035 = EDGE_CURVE('',#6438,#6437,#5395,.T.) ;
#8036 = EDGE_CURVE('',#6424,#6438,#1550,.T.) ;
#8037 = EDGE_CURVE('',#6439,#6438,#5396,.T.) ;
#8038 = EDGE_CURVE('',#6439,#6425,#1551,.T.) ;
#8039 = EDGE_CURVE('',#6440,#6439,#5397,.T.) ;
#8040 = EDGE_CURVE('',#6426,#6440,#1552,.T.) ;
#8041 = EDGE_CURVE('',#6441,#6440,#5398,.T.) ;
#8042 = EDGE_CURVE('',#6441,#6427,#1553,.T.) ;
#8043 = EDGE_CURVE('',#6442,#6441,#5399,.T.) ;
#8044 = EDGE_CURVE('',#6428,#6442,#1554,.T.) ;
#8045 = EDGE_CURVE('',#6443,#6442,#5400,.T.) ;
#8046 = EDGE_CURVE('',#6443,#6429,#1555,.T.) ;
#8047 = EDGE_CURVE('',#6444,#6443,#5401,.T.) ;
#8048 = EDGE_CURVE('',#6430,#6444,#1556,.T.) ;
#8049 = EDGE_CURVE('',#6445,#6444,#5402,.T.) ;
#8050 = EDGE_CURVE('',#6445,#6431,#1557,.T.) ;
#8051 = EDGE_CURVE('',#6446,#6445,#5403,.T.) ;
#8052 = EDGE_CURVE('',#6432,#6446,#1558,.T.) ;
#8053 = EDGE_CURVE('',#6416,#6446,#5404,.T.) ;
#8054 = EDGE_CURVE('',#6447,#6447,#5405,.T.) ;
#8055 = EDGE_CURVE('',#6447,#6448,#1559,.T.) ;
#8056 = EDGE_CURVE('',#6448,#6448,#5406,.T.) ;
#8057 = EDGE_CURVE('',#6449,#6449,#5407,.T.) ;
#8058 = EDGE_CURVE('',#6449,#6450,#1560,.T.) ;
#8059 = EDGE_CURVE('',#6450,#6450,#5408,.T.) ;
#8060 = EDGE_CURVE('',#6451,#6451,#5409,.T.) ;
#8061 = EDGE_CURVE('',#6451,#6452,#1561,.T.) ;
#8062 = EDGE_CURVE('',#6452,#6452,#5410,.T.) ;
#8063 = EDGE_CURVE('',#6453,#6453,#5411,.T.) ;
#8064 = EDGE_CURVE('',#6453,#6454,#1562,.T.) ;
#8065 = EDGE_CURVE('',#6454,#6454,#5412,.T.) ;
#8066 = EDGE_CURVE('',#6455,#6455,#5413,.T.) ;
#8067 = EDGE_CURVE('',#6455,#6456,#1563,.T.) ;
#8068 = EDGE_CURVE('',#6456,#6456,#5414,.T.) ;
#8069 = EDGE_CURVE('',#6457,#6458,#5415,.T.) ;
#8070 = EDGE_CURVE('',#6459,#6457,#1564,.T.) ;
#8071 = EDGE_CURVE('',#6460,#6459,#1565,.T.) ;
#8072 = EDGE_CURVE('',#6458,#6460,#1566,.T.) ;
#8073 = EDGE_CURVE('',#6461,#6457,#1567,.T.) ;
#8074 = EDGE_CURVE('',#6461,#6462,#1568,.T.) ;
#8075 = EDGE_CURVE('',#6462,#6459,#1569,.T.) ;
#8076 = EDGE_CURVE('',#6458,#6463,#1570,.T.) ;
#8077 = EDGE_CURVE('',#6460,#6464,#1571,.T.) ;
#8078 = EDGE_CURVE('',#6464,#6463,#1572,.T.) ;
#8079 = EDGE_CURVE('',#6463,#6461,#5416,.T.) ;
#8080 = EDGE_CURVE('',#6464,#6462,#1573,.T.) ;
#8081 = EDGE_CURVE('',#6465,#6466,#5417,.T.) ;
#8082 = EDGE_CURVE('',#6467,#6465,#1574,.T.) ;
#8083 = EDGE_CURVE('',#6468,#6467,#1575,.T.) ;
#8084 = EDGE_CURVE('',#6466,#6468,#1576,.T.) ;
#8085 = EDGE_CURVE('',#6469,#6465,#1577,.T.) ;
#8086 = EDGE_CURVE('',#6469,#6470,#1578,.T.) ;
#8087 = EDGE_CURVE('',#6470,#6467,#1579,.T.) ;
#8088 = EDGE_CURVE('',#6466,#6471,#1580,.T.) ;
#8089 = EDGE_CURVE('',#6468,#6472,#1581,.T.) ;
#8090 = EDGE_CURVE('',#6472,#6471,#1582,.T.) ;
#8091 = EDGE_CURVE('',#6471,#6469,#5418,.T.) ;
#8092 = EDGE_CURVE('',#6472,#6470,#1583,.T.) ;
#8093 = EDGE_CURVE('',#6473,#6474,#5419,.T.) ;
#8094 = EDGE_CURVE('',#6475,#6473,#1584,.T.) ;
#8095 = EDGE_CURVE('',#6476,#6475,#1585,.T.) ;
#8096 = EDGE_CURVE('',#6474,#6476,#1586,.T.) ;
#8097 = EDGE_CURVE('',#6477,#6473,#1587,.T.) ;
#8098 = EDGE_CURVE('',#6477,#6478,#1588,.T.) ;
#8099 = EDGE_CURVE('',#6478,#6475,#1589,.T.) ;
#8100 = EDGE_CURVE('',#6474,#6479,#1590,.T.) ;
#8101 = EDGE_CURVE('',#6476,#6480,#1591,.T.) ;
#8102 = EDGE_CURVE('',#6480,#6479,#1592,.T.) ;
#8103 = EDGE_CURVE('',#6479,#6477,#5420,.T.) ;
#8104 = EDGE_CURVE('',#6480,#6478,#1593,.T.) ;
#8105 = EDGE_CURVE('',#6481,#6482,#5421,.T.) ;
#8106 = EDGE_CURVE('',#6483,#6481,#1594,.T.) ;
#8107 = EDGE_CURVE('',#6484,#6483,#1595,.T.) ;
#8108 = EDGE_CURVE('',#6482,#6484,#1596,.T.) ;
#8109 = EDGE_CURVE('',#6485,#6481,#1597,.T.) ;
#8110 = EDGE_CURVE('',#6485,#6486,#1598,.T.) ;
#8111 = EDGE_CURVE('',#6486,#6483,#1599,.T.) ;
#8112 = EDGE_CURVE('',#6482,#6487,#1600,.T.) ;
#8113 = EDGE_CURVE('',#6484,#6488,#1601,.T.) ;
#8114 = EDGE_CURVE('',#6488,#6487,#1602,.T.) ;
#8115 = EDGE_CURVE('',#6487,#6485,#5422,.T.) ;
#8116 = EDGE_CURVE('',#6488,#6486,#1603,.T.) ;
#8117 = EDGE_CURVE('',#6489,#6490,#5423,.T.) ;
#8118 = EDGE_CURVE('',#6491,#6489,#1604,.T.) ;
#8119 = EDGE_CURVE('',#6492,#6491,#1605,.T.) ;
#8120 = EDGE_CURVE('',#6493,#6492,#1606,.T.) ;
#8121 = EDGE_CURVE('',#6490,#6493,#5424,.T.) ;
#8122 = EDGE_CURVE('',#6494,#6489,#1607,.T.) ;
#8123 = EDGE_CURVE('',#6494,#6495,#1608,.T.) ;
#8124 = EDGE_CURVE('',#6495,#6491,#1609,.T.) ;
#8125 = EDGE_CURVE('',#6493,#6496,#1610,.T.) ;
#8126 = EDGE_CURVE('',#6492,#6497,#1611,.T.) ;
#8127 = EDGE_CURVE('',#6497,#6496,#1612,.T.) ;
#8128 = EDGE_CURVE('',#6496,#6498,#5425,.T.) ;
#8129 = EDGE_CURVE('',#6497,#6495,#1613,.T.) ;
#8130 = EDGE_CURVE('',#6498,#6494,#5426,.T.) ;
#8131 = EDGE_CURVE('',#6499,#6500,#5427,.T.) ;
#8132 = EDGE_CURVE('',#6501,#6499,#1614,.T.) ;
#8133 = EDGE_CURVE('',#6502,#6501,#1615,.T.) ;
#8134 = EDGE_CURVE('',#6500,#6502,#1616,.T.) ;
#8135 = EDGE_CURVE('',#6503,#6499,#1617,.T.) ;
#8136 = EDGE_CURVE('',#6503,#6504,#1618,.T.) ;
#8137 = EDGE_CURVE('',#6504,#6501,#1619,.T.) ;
#8138 = EDGE_CURVE('',#6500,#6505,#1620,.T.) ;
#8139 = EDGE_CURVE('',#6502,#6506,#1621,.T.) ;
#8140 = EDGE_CURVE('',#6506,#6505,#1622,.T.) ;
#8141 = EDGE_CURVE('',#6505,#6503,#5428,.T.) ;
#8142 = EDGE_CURVE('',#6506,#6504,#1623,.T.) ;
#8143 = EDGE_CURVE('',#6507,#6508,#5429,.T.) ;
#8144 = EDGE_CURVE('',#6509,#6507,#1624,.T.) ;
#8145 = EDGE_CURVE('',#6510,#6509,#1625,.T.) ;
#8146 = EDGE_CURVE('',#6508,#6510,#1626,.T.) ;
#8147 = EDGE_CURVE('',#6511,#6507,#1627,.T.) ;
#8148 = EDGE_CURVE('',#6511,#6512,#1628,.T.) ;
#8149 = EDGE_CURVE('',#6512,#6509,#1629,.T.) ;
#8150 = EDGE_CURVE('',#6508,#6513,#1630,.T.) ;
#8151 = EDGE_CURVE('',#6510,#6514,#1631,.T.) ;
#8152 = EDGE_CURVE('',#6514,#6513,#1632,.T.) ;
#8153 = EDGE_CURVE('',#6513,#6511,#5430,.T.) ;
#8154 = EDGE_CURVE('',#6514,#6512,#1633,.T.) ;
#8155 = EDGE_CURVE('',#6515,#6516,#5431,.T.) ;
#8156 = EDGE_CURVE('',#6517,#6515,#1634,.T.) ;
#8157 = EDGE_CURVE('',#6518,#6517,#1635,.T.) ;
#8158 = EDGE_CURVE('',#6516,#6518,#1636,.T.) ;
#8159 = EDGE_CURVE('',#6519,#6515,#1637,.T.) ;
#8160 = EDGE_CURVE('',#6519,#6520,#1638,.T.) ;
#8161 = EDGE_CURVE('',#6520,#6517,#1639,.T.) ;
#8162 = EDGE_CURVE('',#6516,#6521,#1640,.T.) ;
#8163 = EDGE_CURVE('',#6518,#6522,#1641,.T.) ;
#8164 = EDGE_CURVE('',#6522,#6521,#1642,.T.) ;
#8165 = EDGE_CURVE('',#6521,#6519,#5432,.T.) ;
#8166 = EDGE_CURVE('',#6522,#6520,#1643,.T.) ;
#8167 = EDGE_CURVE('',#6523,#6524,#5433,.T.) ;
#8168 = EDGE_CURVE('',#6525,#6523,#1644,.T.) ;
#8169 = EDGE_CURVE('',#6526,#6525,#1645,.T.) ;
#8170 = EDGE_CURVE('',#6524,#6526,#1646,.T.) ;
#8171 = EDGE_CURVE('',#6527,#6523,#1647,.T.) ;
#8172 = EDGE_CURVE('',#6527,#6528,#1648,.T.) ;
#8173 = EDGE_CURVE('',#6528,#6525,#1649,.T.) ;
#8174 = EDGE_CURVE('',#6524,#6529,#1650,.T.) ;
#8175 = EDGE_CURVE('',#6526,#6530,#1651,.T.) ;
#8176 = EDGE_CURVE('',#6530,#6529,#1652,.T.) ;
#8177 = EDGE_CURVE('',#6529,#6527,#5434,.T.) ;
#8178 = EDGE_CURVE('',#6530,#6528,#1653,.T.) ;
#8179 = EDGE_CURVE('',#6531,#6532,#5435,.T.) ;
#8180 = EDGE_CURVE('',#6533,#6531,#1654,.T.) ;
#8181 = EDGE_CURVE('',#6534,#6533,#1655,.T.) ;
#8182 = EDGE_CURVE('',#6532,#6534,#1656,.T.) ;
#8183 = EDGE_CURVE('',#6535,#6531,#1657,.T.) ;
#8184 = EDGE_CURVE('',#6535,#6536,#1658,.T.) ;
#8185 = EDGE_CURVE('',#6536,#6533,#1659,.T.) ;
#8186 = EDGE_CURVE('',#6532,#6537,#1660,.T.) ;
#8187 = EDGE_CURVE('',#6534,#6538,#1661,.T.) ;
#8188 = EDGE_CURVE('',#6538,#6537,#1662,.T.) ;
#8189 = EDGE_CURVE('',#6537,#6535,#5436,.T.) ;
#8190 = EDGE_CURVE('',#6538,#6536,#1663,.T.) ;
#8191 = EDGE_CURVE('',#6539,#6539,#5437,.T.) ;
#8192 = EDGE_CURVE('',#6539,#6498,#1664,.T.) ;
#8193 = EDGE_CURVE('',#6490,#6540,#1665,.T.) ;
#8194 = EDGE_CURVE('',#6540,#6540,#5438,.T.) ;
#8195 = EDGE_CURVE('',#6541,#6541,#5439,.T.) ;
#8196 = EDGE_CURVE('',#6541,#6542,#1666,.T.) ;
#8197 = EDGE_CURVE('',#6542,#6542,#5440,.T.) ;
#8198 = EDGE_CURVE('',#6543,#6543,#5441,.T.) ;
#8199 = EDGE_CURVE('',#6543,#6544,#1667,.T.) ;
#8200 = EDGE_CURVE('',#6544,#6544,#5442,.T.) ;
#8201 = EDGE_CURVE('',#6545,#6546,#1668,.T.) ;
#8202 = EDGE_CURVE('',#6545,#6547,#5443,.T.) ;
#8203 = EDGE_CURVE('',#6548,#6547,#1669,.T.) ;
#8204 = EDGE_CURVE('',#6548,#6546,#5444,.T.) ;
#8205 = EDGE_CURVE('',#6549,#6549,#5445,.T.) ;
#8206 = EDGE_CURVE('',#6549,#6547,#1670,.T.) ;
#8207 = EDGE_CURVE('',#6547,#6545,#353,.T.) ;
#8208 = EDGE_CURVE('',#6546,#6550,#1671,.T.) ;
#8209 = EDGE_CURVE('',#6551,#6548,#1672,.T.) ;
#8210 = EDGE_CURVE('',#6551,#6552,#1673,.T.) ;
#8211 = EDGE_CURVE('',#6552,#6552,#5446,.T.) ;
#8212 = EDGE_CURVE('',#6550,#6551,#984,.T.) ;
#8213 = EDGE_CURVE('',#6547,#6545,#5447,.T.) ;
#8214 = EDGE_CURVE('',#6547,#6553,#1674,.T.) ;
#8215 = EDGE_CURVE('',#6554,#6553,#354,.T.) ;
#8216 = EDGE_CURVE('',#6555,#6554,#5448,.T.) ;
#8217 = EDGE_CURVE('',#6553,#6555,#355,.T.) ;
#8218 = EDGE_CURVE('',#6550,#6551,#5449,.T.) ;
#8219 = EDGE_CURVE('',#6556,#6556,#5450,.T.) ;
#8220 = EDGE_CURVE('',#6554,#6555,#5451,.T.) ;
#8221 = EDGE_CURVE('',#6557,#6558,#5452,.T.) ;
#8222 = EDGE_CURVE('',#6558,#6559,#5453,.T.) ;
#8223 = EDGE_CURVE('',#6558,#6560,#5454,.T.) ;
#8224 = EDGE_CURVE('',#6560,#6561,#5455,.T.) ;
#8225 = EDGE_CURVE('',#6561,#6557,#5456,.T.) ;
#8226 = EDGE_CURVE('',#6562,#6563,#5457,.T.) ;
#8227 = EDGE_CURVE('',#6563,#6562,#5458,.T.) ;
#8228 = EDGE_CURVE('',#6553,#6564,#1675,.T.) ;
#8229 = EDGE_CURVE('',#6560,#6564,#356,.T.) ;
#8230 = EDGE_CURVE('',#6564,#6557,#357,.T.) ;
#8231 = EDGE_CURVE('',#6561,#6563,#1676,.T.) ;
#8232 = EDGE_CURVE('',#6563,#6562,#358,.T.) ;
#8233 = EDGE_CURVE('',#6556,#6565,#1677,.T.) ;
#8234 = EDGE_CURVE('',#6565,#6565,#5459,.T.) ;
#8235 = EDGE_CURVE('',#6566,#6566,#5460,.T.) ;
#8236 = EDGE_CURVE('',#6566,#6563,#1678,.T.) ;
#8237 = EDGE_CURVE('',#6567,#6568,#1679,.T.) ;
#8238 = EDGE_CURVE('',#6569,#6567,#1680,.T.) ;
#8239 = EDGE_CURVE('',#6570,#6569,#1681,.T.) ;
#8240 = EDGE_CURVE('',#6568,#6570,#1682,.T.) ;
#8241 = EDGE_CURVE('',#6571,#6572,#1683,.T.) ;
#8242 = EDGE_CURVE('',#6573,#6571,#1684,.T.) ;
#8243 = EDGE_CURVE('',#6574,#6573,#1685,.T.) ;
#8244 = EDGE_CURVE('',#6572,#6574,#1686,.T.) ;
#8245 = EDGE_CURVE('',#6575,#6576,#1687,.T.) ;
#8246 = EDGE_CURVE('',#6577,#6575,#1688,.T.) ;
#8247 = EDGE_CURVE('',#6577,#6578,#1689,.T.) ;
#8248 = EDGE_CURVE('',#6576,#6578,#1690,.T.) ;
#8249 = EDGE_CURVE('',#6578,#6569,#1691,.T.) ;
#8250 = EDGE_CURVE('',#6570,#6577,#1692,.T.) ;
#8251 = EDGE_CURVE('',#6567,#6576,#5461,.T.) ;
#8252 = EDGE_CURVE('',#6574,#6572,#5462,.T.) ;
#8253 = EDGE_CURVE('',#6571,#6573,#5463,.T.) ;
#8254 = EDGE_CURVE('',#6575,#6568,#5464,.T.) ;
#8255 = EDGE_CURVE('',#6579,#6580,#1693,.T.) ;
#8256 = EDGE_CURVE('',#6579,#6581,#1694,.T.) ;
#8257 = EDGE_CURVE('',#6581,#6582,#1695,.T.) ;
#8258 = EDGE_CURVE('',#6582,#6580,#1696,.T.) ;
#8259 = EDGE_CURVE('',#6583,#6584,#1697,.T.) ;
#8260 = EDGE_CURVE('',#6585,#6583,#1698,.T.) ;
#8261 = EDGE_CURVE('',#6586,#6585,#1699,.T.) ;
#8262 = EDGE_CURVE('',#6586,#6584,#1700,.T.) ;
#8263 = EDGE_CURVE('',#6587,#6588,#1701,.T.) ;
#8264 = EDGE_CURVE('',#6587,#6589,#1702,.T.) ;
#8265 = EDGE_CURVE('',#6589,#6590,#1703,.T.) ;
#8266 = EDGE_CURVE('',#6590,#6588,#1704,.T.) ;
#8267 = EDGE_CURVE('',#6581,#6590,#1705,.T.) ;
#8268 = EDGE_CURVE('',#6582,#6589,#1706,.T.) ;
#8269 = EDGE_CURVE('',#6579,#6588,#5465,.T.) ;
#8270 = EDGE_CURVE('',#6587,#6580,#5466,.T.) ;
#8271 = EDGE_CURVE('',#6586,#6584,#5467,.T.) ;
#8272 = EDGE_CURVE('',#6583,#6585,#5468,.T.) ;
#8273 = EDGE_CURVE('',#6591,#6592,#985,.T.) ;
#8274 = EDGE_CURVE('',#6593,#6591,#986,.T.) ;
#8275 = EDGE_CURVE('',#6593,#6594,#1707,.T.) ;
#8276 = EDGE_CURVE('',#6595,#6594,#987,.T.) ;
#8277 = EDGE_CURVE('',#6596,#6595,#988,.T.) ;
#8278 = EDGE_CURVE('',#6594,#6596,#989,.T.) ;
#8279 = EDGE_CURVE('',#6592,#6593,#990,.T.) ;
#8280 = EDGE_CURVE('',#6597,#6597,#5469,.T.) ;
#8281 = EDGE_CURVE('',#6597,#6593,#1708,.T.) ;
#8282 = EDGE_CURVE('',#6592,#6598,#1709,.T.) ;
#8283 = EDGE_CURVE('',#6598,#6598,#5470,.T.) ;
#8284 = EDGE_CURVE('',#6599,#6599,#5471,.T.) ;
#8285 = EDGE_CURVE('',#6599,#6596,#1710,.T.) ;
#8286 = EDGE_CURVE('',#6594,#6600,#1711,.T.) ;
#8287 = EDGE_CURVE('',#6600,#6600,#5472,.T.) ;
#8288 = EDGE_CURVE('',#6601,#6602,#1712,.T.) ;
#8289 = EDGE_CURVE('',#6603,#6601,#5473,.T.) ;
#8290 = EDGE_CURVE('',#6604,#6603,#1713,.T.) ;
#8291 = EDGE_CURVE('',#6602,#6604,#5474,.T.) ;
#8292 = EDGE_CURVE('',#6602,#6605,#991,.T.) ;
#8293 = EDGE_CURVE('',#6606,#6604,#992,.T.) ;
#8294 = EDGE_CURVE('',#6607,#6606,#993,.T.) ;
#8295 = EDGE_CURVE('',#6607,#6608,#5475,.T.) ;
#8296 = EDGE_CURVE('',#6605,#6608,#994,.T.) ;
#8297 = EDGE_CURVE('',#6609,#6610,#995,.T.) ;
#8298 = EDGE_CURVE('',#6609,#6611,#5476,.T.) ;
#8299 = EDGE_CURVE('',#6612,#6611,#996,.T.) ;
#8300 = EDGE_CURVE('',#6603,#6612,#997,.T.) ;
#8301 = EDGE_CURVE('',#6610,#6601,#998,.T.) ;
#8302 = EDGE_CURVE('',#6608,#6609,#1714,.T.) ;
#8303 = EDGE_CURVE('',#6611,#6607,#1715,.T.) ;
#8304 = EDGE_CURVE('',#6613,#6613,#5477,.T.) ;
#8305 = EDGE_CURVE('',#6613,#6605,#1716,.T.) ;
#8306 = EDGE_CURVE('',#6610,#6614,#1717,.T.) ;
#8307 = EDGE_CURVE('',#6614,#6614,#5478,.T.) ;
#8308 = EDGE_CURVE('',#6615,#6615,#5479,.T.) ;
#8309 = EDGE_CURVE('',#6615,#6616,#1718,.T.) ;
#8310 = EDGE_CURVE('',#6616,#6616,#5480,.T.) ;
#8311 = EDGE_CURVE('',#6616,#6612,#1719,.T.) ;
#8312 = EDGE_CURVE('',#6606,#6617,#1720,.T.) ;
#8313 = EDGE_CURVE('',#6617,#6617,#5481,.T.) ;
#8314 = EDGE_CURVE('',#6617,#6618,#1721,.T.) ;
#8315 = EDGE_CURVE('',#6618,#6618,#5482,.T.) ;
#8316 = EDGE_CURVE('',#6619,#6619,#5483,.T.) ;
#8317 = EDGE_CURVE('',#6619,#6620,#1722,.T.) ;
#8318 = EDGE_CURVE('',#6620,#6620,#5484,.T.) ;
#8319 = EDGE_CURVE('',#6621,#6621,#5485,.T.) ;
#8320 = EDGE_CURVE('',#6621,#6622,#1723,.T.) ;
#8321 = EDGE_CURVE('',#6622,#6622,#5486,.T.) ;
#8322 = EDGE_CURVE('',#6623,#6623,#5487,.T.) ;
#8323 = EDGE_CURVE('',#6623,#6624,#1724,.T.) ;
#8324 = EDGE_CURVE('',#6624,#6624,#5488,.T.) ;
#8325 = EDGE_CURVE('',#6625,#6625,#5489,.T.) ;
#8326 = EDGE_CURVE('',#6625,#6626,#1725,.T.) ;
#8327 = EDGE_CURVE('',#6626,#6626,#5490,.T.) ;
#8328 = EDGE_CURVE('',#6627,#6627,#5491,.T.) ;
#8329 = EDGE_CURVE('',#6627,#6628,#1726,.T.) ;
#8330 = EDGE_CURVE('',#6628,#6628,#5492,.T.) ;
#8331 = EDGE_CURVE('',#6629,#6629,#5493,.T.) ;
#8332 = EDGE_CURVE('',#6629,#6630,#1727,.T.) ;
#8333 = EDGE_CURVE('',#6630,#6630,#5494,.T.) ;
#8334 = EDGE_CURVE('',#6631,#6631,#5495,.T.) ;
#8335 = EDGE_CURVE('',#6631,#6632,#1728,.T.) ;
#8336 = EDGE_CURVE('',#6632,#6632,#5496,.T.) ;
#8337 = EDGE_CURVE('',#6633,#6633,#5497,.T.) ;
#8338 = EDGE_CURVE('',#6633,#6634,#1729,.T.) ;
#8339 = EDGE_CURVE('',#6634,#6634,#5498,.T.) ;
#8340 = EDGE_CURVE('',#6635,#6635,#5499,.T.) ;
#8341 = EDGE_CURVE('',#6635,#6636,#1730,.T.) ;
#8342 = EDGE_CURVE('',#6636,#6636,#5500,.T.) ;
#8343 = EDGE_CURVE('',#6637,#6637,#5501,.T.) ;
#8344 = EDGE_CURVE('',#6637,#6638,#1731,.T.) ;
#8345 = EDGE_CURVE('',#6638,#6638,#5502,.T.) ;
#8346 = EDGE_CURVE('',#6639,#6639,#5503,.T.) ;
#8347 = EDGE_CURVE('',#6639,#6640,#1732,.T.) ;
#8348 = EDGE_CURVE('',#6640,#6640,#5504,.T.) ;
#8349 = EDGE_CURVE('',#6641,#6641,#5505,.T.) ;
#8350 = EDGE_CURVE('',#6641,#6642,#1733,.T.) ;
#8351 = EDGE_CURVE('',#6642,#6642,#5506,.T.) ;
#8352 = EDGE_CURVE('',#6643,#6643,#5507,.T.) ;
#8353 = EDGE_CURVE('',#6643,#6644,#1734,.T.) ;
#8354 = EDGE_CURVE('',#6644,#6644,#5508,.T.) ;
#8355 = EDGE_CURVE('',#6645,#6645,#5509,.T.) ;
#8356 = EDGE_CURVE('',#6645,#6646,#1735,.T.) ;
#8357 = EDGE_CURVE('',#6646,#6646,#5510,.T.) ;
#8358 = EDGE_CURVE('',#6647,#6648,#1736,.T.) ;
#8359 = EDGE_CURVE('',#6648,#6647,#5511,.T.) ;
#8360 = EDGE_CURVE('',#6649,#6649,#5512,.T.) ;
#8361 = EDGE_CURVE('',#6649,#6650,#1737,.T.) ;
#8362 = EDGE_CURVE('',#6650,#6650,#5513,.T.) ;
#8363 = EDGE_CURVE('',#6648,#6647,#999,.T.) ;
#8364 = EDGE_CURVE('',#6651,#6652,#1738,.T.) ;
#8365 = EDGE_CURVE('',#6652,#6651,#5514,.T.) ;
#8366 = EDGE_CURVE('',#6653,#6653,#5515,.T.) ;
#8367 = EDGE_CURVE('',#6653,#6654,#1739,.T.) ;
#8368 = EDGE_CURVE('',#6654,#6654,#5516,.T.) ;
#8369 = EDGE_CURVE('',#6652,#6651,#1000,.T.) ;
#8370 = EDGE_CURVE('',#6655,#6656,#1740,.T.) ;
#8371 = EDGE_CURVE('',#6655,#6657,#1741,.T.) ;
#8372 = EDGE_CURVE('',#6657,#6658,#1742,.T.) ;
#8373 = EDGE_CURVE('',#6658,#6656,#1743,.T.) ;
#8374 = EDGE_CURVE('',#6659,#6660,#1744,.T.) ;
#8375 = EDGE_CURVE('',#6659,#6661,#1745,.T.) ;
#8376 = EDGE_CURVE('',#6661,#6662,#1746,.T.) ;
#8377 = EDGE_CURVE('',#6662,#6660,#1747,.T.) ;
#8378 = EDGE_CURVE('',#6663,#6664,#1748,.T.) ;
#8379 = EDGE_CURVE('',#6664,#6665,#1749,.T.) ;
#8380 = EDGE_CURVE('',#6665,#6666,#1750,.T.) ;
#8381 = EDGE_CURVE('',#6666,#6663,#1751,.T.) ;
#8382 = EDGE_CURVE('',#6657,#6665,#1752,.T.) ;
#8383 = EDGE_CURVE('',#6658,#6664,#1753,.T.) ;
#8384 = EDGE_CURVE('',#6661,#6663,#1754,.T.) ;
#8385 = EDGE_CURVE('',#6662,#6666,#1755,.T.) ;
#8386 = EDGE_CURVE('',#6655,#6660,#5517,.T.) ;
#8387 = EDGE_CURVE('',#6667,#6667,#5518,.T.) ;
#8388 = EDGE_CURVE('',#6659,#6656,#5519,.T.) ;
#8389 = EDGE_CURVE('',#6667,#6668,#1756,.T.) ;
#8390 = EDGE_CURVE('',#6668,#6668,#5520,.T.) ;
#8391 = EDGE_CURVE('',#6669,#6669,#5521,.T.) ;
#8392 = EDGE_CURVE('',#6669,#6670,#1757,.T.) ;
#8393 = EDGE_CURVE('',#6670,#6670,#5522,.T.) ;
#8394 = EDGE_CURVE('',#6671,#6671,#5523,.T.) ;
#8395 = EDGE_CURVE('',#6671,#6672,#1758,.T.) ;
#8396 = EDGE_CURVE('',#6672,#6672,#5524,.T.) ;
#8397 = EDGE_CURVE('',#6673,#6673,#5525,.T.) ;
#8398 = EDGE_CURVE('',#6673,#6674,#1759,.T.) ;
#8399 = EDGE_CURVE('',#6674,#6674,#5526,.T.) ;
#8400 = EDGE_CURVE('',#6675,#6675,#5527,.T.) ;
#8401 = EDGE_CURVE('',#6675,#6676,#1760,.T.) ;
#8402 = EDGE_CURVE('',#6676,#6676,#5528,.T.) ;
#8403 = EDGE_CURVE('',#6677,#6677,#5529,.T.) ;
#8404 = EDGE_CURVE('',#6677,#6678,#1761,.T.) ;
#8405 = EDGE_CURVE('',#6678,#6678,#5530,.T.) ;
#8406 = EDGE_CURVE('',#6679,#6680,#1762,.T.) ;
#8407 = EDGE_CURVE('',#6679,#6681,#1763,.T.) ;
#8408 = EDGE_CURVE('',#6682,#6681,#1764,.T.) ;
#8409 = EDGE_CURVE('',#6682,#6680,#1765,.T.) ;
#8410 = EDGE_CURVE('',#6683,#6684,#1766,.T.) ;
#8411 = EDGE_CURVE('',#6683,#6685,#1767,.T.) ;
#8412 = EDGE_CURVE('',#6686,#6685,#1768,.T.) ;
#8413 = EDGE_CURVE('',#6686,#6684,#1769,.T.) ;
#8414 = EDGE_CURVE('',#6687,#6679,#1770,.T.) ;
#8415 = EDGE_CURVE('',#6685,#6687,#1771,.T.) ;
#8416 = EDGE_CURVE('',#6688,#6683,#1772,.T.) ;
#8417 = EDGE_CURVE('',#6681,#6688,#1773,.T.) ;
#8418 = EDGE_CURVE('',#6687,#6689,#1774,.T.) ;
#8419 = EDGE_CURVE('',#6680,#6689,#1775,.T.) ;
#8420 = EDGE_CURVE('',#6688,#6690,#1776,.T.) ;
#8421 = EDGE_CURVE('',#6684,#6690,#1777,.T.) ;
#8422 = EDGE_CURVE('',#6689,#6686,#1778,.T.) ;
#8423 = EDGE_CURVE('',#6690,#6682,#1779,.T.) ;
#8424 = EDGE_CURVE('',#6691,#6691,#5531,.T.) ;
#8425 = EDGE_CURVE('',#6691,#6692,#1780,.T.) ;
#8426 = EDGE_CURVE('',#6692,#6692,#5532,.T.) ;
#8427 = EDGE_CURVE('',#6693,#6694,#1781,.T.) ;
#8428 = EDGE_CURVE('',#6693,#6695,#1782,.T.) ;
#8429 = EDGE_CURVE('',#6696,#6695,#1783,.T.) ;
#8430 = EDGE_CURVE('',#6696,#6694,#1784,.T.) ;
#8431 = EDGE_CURVE('',#6697,#6698,#1785,.T.) ;
#8432 = EDGE_CURVE('',#6697,#6699,#1786,.T.) ;
#8433 = EDGE_CURVE('',#6700,#6699,#1787,.T.) ;
#8434 = EDGE_CURVE('',#6700,#6698,#1788,.T.) ;
#8435 = EDGE_CURVE('',#6701,#6693,#1789,.T.) ;
#8436 = EDGE_CURVE('',#6699,#6701,#1790,.T.) ;
#8437 = EDGE_CURVE('',#6702,#6697,#1791,.T.) ;
#8438 = EDGE_CURVE('',#6695,#6702,#1792,.T.) ;
#8439 = EDGE_CURVE('',#6701,#6703,#1793,.T.) ;
#8440 = EDGE_CURVE('',#6694,#6703,#1794,.T.) ;
#8441 = EDGE_CURVE('',#6702,#6704,#1795,.T.) ;
#8442 = EDGE_CURVE('',#6698,#6704,#1796,.T.) ;
#8443 = EDGE_CURVE('',#6703,#6700,#1797,.T.) ;
#8444 = EDGE_CURVE('',#6704,#6696,#1798,.T.) ;
#8445 = EDGE_CURVE('',#6705,#6705,#5533,.T.) ;
#8446 = EDGE_CURVE('',#6705,#6706,#1799,.T.) ;
#8447 = EDGE_CURVE('',#6706,#6706,#5534,.T.) ;
#8448 = EDGE_CURVE('',#6707,#6708,#1800,.T.) ;
#8449 = EDGE_CURVE('',#6707,#6709,#1801,.T.) ;
#8450 = EDGE_CURVE('',#6710,#6709,#1802,.T.) ;
#8451 = EDGE_CURVE('',#6710,#6708,#1803,.T.) ;
#8452 = EDGE_CURVE('',#6711,#6712,#1804,.T.) ;
#8453 = EDGE_CURVE('',#6711,#6713,#1805,.T.) ;
#8454 = EDGE_CURVE('',#6714,#6713,#1806,.T.) ;
#8455 = EDGE_CURVE('',#6714,#6712,#1807,.T.) ;
#8456 = EDGE_CURVE('',#6715,#6707,#1808,.T.) ;
#8457 = EDGE_CURVE('',#6713,#6715,#1809,.T.) ;
#8458 = EDGE_CURVE('',#6716,#6711,#1810,.T.) ;
#8459 = EDGE_CURVE('',#6709,#6716,#1811,.T.) ;
#8460 = EDGE_CURVE('',#6715,#6717,#1812,.T.) ;
#8461 = EDGE_CURVE('',#6708,#6717,#1813,.T.) ;
#8462 = EDGE_CURVE('',#6716,#6718,#1814,.T.) ;
#8463 = EDGE_CURVE('',#6712,#6718,#1815,.T.) ;
#8464 = EDGE_CURVE('',#6717,#6714,#1816,.T.) ;
#8465 = EDGE_CURVE('',#6718,#6710,#1817,.T.) ;
#8466 = EDGE_CURVE('',#6719,#6719,#5535,.T.) ;
#8467 = EDGE_CURVE('',#6719,#6720,#1818,.T.) ;
#8468 = EDGE_CURVE('',#6720,#6720,#5536,.T.) ;
#8469 = EDGE_CURVE('',#6721,#6722,#1819,.T.) ;
#8470 = EDGE_CURVE('',#6721,#6723,#1820,.T.) ;
#8471 = EDGE_CURVE('',#6724,#6723,#1821,.T.) ;
#8472 = EDGE_CURVE('',#6724,#6722,#1822,.T.) ;
#8473 = EDGE_CURVE('',#6725,#6726,#1823,.T.) ;
#8474 = EDGE_CURVE('',#6725,#6727,#1824,.T.) ;
#8475 = EDGE_CURVE('',#6728,#6727,#1825,.T.) ;
#8476 = EDGE_CURVE('',#6728,#6726,#1826,.T.) ;
#8477 = EDGE_CURVE('',#6729,#6721,#1827,.T.) ;
#8478 = EDGE_CURVE('',#6727,#6729,#1828,.T.) ;
#8479 = EDGE_CURVE('',#6730,#6725,#1829,.T.) ;
#8480 = EDGE_CURVE('',#6723,#6730,#1830,.T.) ;
#8481 = EDGE_CURVE('',#6729,#6731,#1831,.T.) ;
#8482 = EDGE_CURVE('',#6722,#6731,#1832,.T.) ;
#8483 = EDGE_CURVE('',#6730,#6732,#1833,.T.) ;
#8484 = EDGE_CURVE('',#6726,#6732,#1834,.T.) ;
#8485 = EDGE_CURVE('',#6731,#6728,#1835,.T.) ;
#8486 = EDGE_CURVE('',#6732,#6724,#1836,.T.) ;
#8487 = ORIENTED_EDGE('',*,*,#6733,.F.) ;
#8488 = ORIENTED_EDGE('',*,*,#6734,.F.) ;
#8489 = ORIENTED_EDGE('',*,*,#6735,.F.) ;
#8490 = ORIENTED_EDGE('',*,*,#6736,.F.) ;
#8491 = ORIENTED_EDGE('',*,*,#6737,.T.) ;
#8492 = ORIENTED_EDGE('',*,*,#6734,.T.) ;
#8493 = ORIENTED_EDGE('',*,*,#6738,.F.) ;
#8494 = ORIENTED_EDGE('',*,*,#6739,.F.) ;
#8495 = ORIENTED_EDGE('',*,*,#6740,.F.) ;
#8496 = ORIENTED_EDGE('',*,*,#6735,.T.) ;
#8497 = ORIENTED_EDGE('',*,*,#6737,.F.) ;
#8498 = ORIENTED_EDGE('',*,*,#6738,.T.) ;
#8499 = ORIENTED_EDGE('',*,*,#6733,.T.) ;
#8500 = ORIENTED_EDGE('',*,*,#6740,.T.) ;
#8501 = ORIENTED_EDGE('',*,*,#6741,.T.) ;
#8502 = ORIENTED_EDGE('',*,*,#6742,.T.) ;
#8503 = ORIENTED_EDGE('',*,*,#6743,.T.) ;
#8504 = ORIENTED_EDGE('',*,*,#6744,.T.) ;
#8505 = ORIENTED_EDGE('',*,*,#6745,.T.) ;
#8506 = ORIENTED_EDGE('',*,*,#6746,.T.) ;
#8507 = ORIENTED_EDGE('',*,*,#6747,.F.) ;
#8508 = ORIENTED_EDGE('',*,*,#6746,.F.) ;
#8509 = ORIENTED_EDGE('',*,*,#6748,.T.) ;
#8510 = ORIENTED_EDGE('',*,*,#6749,.T.) ;
#8511 = ORIENTED_EDGE('',*,*,#6750,.T.) ;
#8512 = ORIENTED_EDGE('',*,*,#6751,.T.) ;
#8513 = ORIENTED_EDGE('',*,*,#6752,.T.) ;
#8514 = ORIENTED_EDGE('',*,*,#6753,.T.) ;
#8515 = ORIENTED_EDGE('',*,*,#6754,.T.) ;
#8516 = ORIENTED_EDGE('',*,*,#6755,.T.) ;
#8517 = ORIENTED_EDGE('',*,*,#6756,.T.) ;
#8518 = ORIENTED_EDGE('',*,*,#6757,.T.) ;
#8519 = ORIENTED_EDGE('',*,*,#6758,.F.) ;
#8520 = ORIENTED_EDGE('',*,*,#6759,.T.) ;
#8521 = ORIENTED_EDGE('',*,*,#6760,.T.) ;
#8522 = ORIENTED_EDGE('',*,*,#6742,.F.) ;
#8523 = ORIENTED_EDGE('',*,*,#6761,.F.) ;
#8524 = ORIENTED_EDGE('',*,*,#6744,.F.) ;
#8525 = ORIENTED_EDGE('',*,*,#6762,.T.) ;
#8526 = ORIENTED_EDGE('',*,*,#6759,.F.) ;
#8527 = ORIENTED_EDGE('',*,*,#6743,.F.) ;
#8528 = ORIENTED_EDGE('',*,*,#6760,.F.) ;
#8529 = ORIENTED_EDGE('',*,*,#6762,.F.) ;
#8530 = ORIENTED_EDGE('',*,*,#6739,.T.) ;
#8531 = ORIENTED_EDGE('',*,*,#6752,.F.) ;
#8532 = ORIENTED_EDGE('',*,*,#6763,.T.) ;
#8533 = ORIENTED_EDGE('',*,*,#6764,.T.) ;
#8534 = ORIENTED_EDGE('',*,*,#6748,.F.) ;
#8535 = ORIENTED_EDGE('',*,*,#6745,.F.) ;
#8536 = ORIENTED_EDGE('',*,*,#6761,.T.) ;
#8537 = ORIENTED_EDGE('',*,*,#6741,.F.) ;
#8538 = ORIENTED_EDGE('',*,*,#6765,.T.) ;
#8539 = ORIENTED_EDGE('',*,*,#6766,.F.) ;
#8540 = ORIENTED_EDGE('',*,*,#6767,.T.) ;
#8541 = ORIENTED_EDGE('',*,*,#6768,.F.) ;
#8542 = ORIENTED_EDGE('',*,*,#6767,.F.) ;
#8543 = ORIENTED_EDGE('',*,*,#6769,.F.) ;
#8544 = ORIENTED_EDGE('',*,*,#6770,.T.) ;
#8545 = ORIENTED_EDGE('',*,*,#6771,.F.) ;
#8546 = ORIENTED_EDGE('',*,*,#6770,.F.) ;
#8547 = ORIENTED_EDGE('',*,*,#6772,.F.) ;
#8548 = ORIENTED_EDGE('',*,*,#6773,.T.) ;
#8549 = ORIENTED_EDGE('',*,*,#6774,.F.) ;
#8550 = ORIENTED_EDGE('',*,*,#6773,.F.) ;
#8551 = ORIENTED_EDGE('',*,*,#6775,.F.) ;
#8552 = ORIENTED_EDGE('',*,*,#6776,.T.) ;
#8553 = ORIENTED_EDGE('',*,*,#6777,.F.) ;
#8554 = ORIENTED_EDGE('',*,*,#6776,.F.) ;
#8555 = ORIENTED_EDGE('',*,*,#6778,.F.) ;
#8556 = ORIENTED_EDGE('',*,*,#6779,.T.) ;
#8557 = ORIENTED_EDGE('',*,*,#6780,.F.) ;
#8558 = ORIENTED_EDGE('',*,*,#6779,.F.) ;
#8559 = ORIENTED_EDGE('',*,*,#6781,.F.) ;
#8560 = ORIENTED_EDGE('',*,*,#6782,.T.) ;
#8561 = ORIENTED_EDGE('',*,*,#6783,.F.) ;
#8562 = ORIENTED_EDGE('',*,*,#6782,.F.) ;
#8563 = ORIENTED_EDGE('',*,*,#6784,.F.) ;
#8564 = ORIENTED_EDGE('',*,*,#6785,.F.) ;
#8565 = ORIENTED_EDGE('',*,*,#6786,.F.) ;
#8566 = ORIENTED_EDGE('',*,*,#6787,.F.) ;
#8567 = ORIENTED_EDGE('',*,*,#6788,.F.) ;
#8568 = ORIENTED_EDGE('',*,*,#6789,.T.) ;
#8569 = ORIENTED_EDGE('',*,*,#6790,.F.) ;
#8570 = ORIENTED_EDGE('',*,*,#6791,.T.) ;
#8571 = ORIENTED_EDGE('',*,*,#6792,.T.) ;
#8572 = ORIENTED_EDGE('',*,*,#6786,.T.) ;
#8573 = ORIENTED_EDGE('',*,*,#6793,.F.) ;
#8574 = ORIENTED_EDGE('',*,*,#6789,.F.) ;
#8575 = ORIENTED_EDGE('',*,*,#6794,.F.) ;
#8576 = ORIENTED_EDGE('',*,*,#6795,.T.) ;
#8577 = ORIENTED_EDGE('',*,*,#6796,.T.) ;
#8578 = ORIENTED_EDGE('',*,*,#6794,.T.) ;
#8579 = ORIENTED_EDGE('',*,*,#6788,.T.) ;
#8580 = ORIENTED_EDGE('',*,*,#6797,.T.) ;
#8581 = ORIENTED_EDGE('',*,*,#6787,.T.) ;
#8582 = ORIENTED_EDGE('',*,*,#6792,.F.) ;
#8583 = ORIENTED_EDGE('',*,*,#6798,.F.) ;
#8584 = ORIENTED_EDGE('',*,*,#6797,.F.) ;
#8585 = ORIENTED_EDGE('',*,*,#6736,.T.) ;
#8586 = ORIENTED_EDGE('',*,*,#6758,.T.) ;
#8587 = ORIENTED_EDGE('',*,*,#6799,.F.) ;
#8588 = ORIENTED_EDGE('',*,*,#6796,.F.) ;
#8589 = ORIENTED_EDGE('',*,*,#6800,.T.) ;
#8590 = ORIENTED_EDGE('',*,*,#6801,.F.) ;
#8591 = ORIENTED_EDGE('',*,*,#6800,.F.) ;
#8592 = ORIENTED_EDGE('',*,*,#6795,.F.) ;
#8593 = ORIENTED_EDGE('',*,*,#6798,.T.) ;
#8594 = ORIENTED_EDGE('',*,*,#6791,.F.) ;
#8595 = ORIENTED_EDGE('',*,*,#6802,.F.) ;
#8596 = ORIENTED_EDGE('',*,*,#6803,.F.) ;
#8597 = ORIENTED_EDGE('',*,*,#6804,.T.) ;
#8598 = ORIENTED_EDGE('',*,*,#6805,.F.) ;
#8599 = ORIENTED_EDGE('',*,*,#6784,.T.) ;
#8600 = ORIENTED_EDGE('',*,*,#6793,.T.) ;
#8601 = ORIENTED_EDGE('',*,*,#6799,.T.) ;
#8602 = ORIENTED_EDGE('',*,*,#6801,.T.) ;
#8603 = ORIENTED_EDGE('',*,*,#6806,.F.) ;
#8604 = ORIENTED_EDGE('',*,*,#6807,.T.) ;
#8605 = ORIENTED_EDGE('',*,*,#6808,.T.) ;
#8606 = ORIENTED_EDGE('',*,*,#6809,.T.) ;
#8607 = ORIENTED_EDGE('',*,*,#6810,.F.) ;
#8608 = ORIENTED_EDGE('',*,*,#6804,.F.) ;
#8609 = ORIENTED_EDGE('',*,*,#6811,.T.) ;
#8610 = ORIENTED_EDGE('',*,*,#6812,.T.) ;
#8611 = ORIENTED_EDGE('',*,*,#6813,.F.) ;
#8612 = ORIENTED_EDGE('',*,*,#6814,.T.) ;
#8613 = ORIENTED_EDGE('',*,*,#6753,.F.) ;
#8614 = ORIENTED_EDGE('',*,*,#6815,.F.) ;
#8615 = ORIENTED_EDGE('',*,*,#6754,.F.) ;
#8616 = ORIENTED_EDGE('',*,*,#6814,.F.) ;
#8617 = ORIENTED_EDGE('',*,*,#6811,.F.) ;
#8618 = ORIENTED_EDGE('',*,*,#6812,.F.) ;
#8619 = ORIENTED_EDGE('',*,*,#6816,.T.) ;
#8620 = ORIENTED_EDGE('',*,*,#6817,.F.) ;
#8621 = ORIENTED_EDGE('',*,*,#6816,.F.) ;
#8622 = ORIENTED_EDGE('',*,*,#6756,.F.) ;
#8623 = ORIENTED_EDGE('',*,*,#6818,.F.) ;
#8624 = ORIENTED_EDGE('',*,*,#6817,.T.) ;
#8625 = ORIENTED_EDGE('',*,*,#6813,.T.) ;
#8626 = ORIENTED_EDGE('',*,*,#6815,.T.) ;
#8627 = ORIENTED_EDGE('',*,*,#6757,.F.) ;
#8628 = ORIENTED_EDGE('',*,*,#6818,.T.) ;
#8629 = ORIENTED_EDGE('',*,*,#6755,.F.) ;
#8630 = ORIENTED_EDGE('',*,*,#6750,.F.) ;
#8631 = ORIENTED_EDGE('',*,*,#6819,.F.) ;
#8632 = ORIENTED_EDGE('',*,*,#6820,.F.) ;
#8633 = ORIENTED_EDGE('',*,*,#6821,.T.) ;
#8634 = ORIENTED_EDGE('',*,*,#6763,.F.) ;
#8635 = ORIENTED_EDGE('',*,*,#6751,.F.) ;
#8636 = ORIENTED_EDGE('',*,*,#6819,.T.) ;
#8637 = ORIENTED_EDGE('',*,*,#6749,.F.) ;
#8638 = ORIENTED_EDGE('',*,*,#6764,.F.) ;
#8639 = ORIENTED_EDGE('',*,*,#6821,.F.) ;
#8640 = ORIENTED_EDGE('',*,*,#6808,.F.) ;
#8641 = ORIENTED_EDGE('',*,*,#6822,.T.) ;
#8642 = ORIENTED_EDGE('',*,*,#6809,.F.) ;
#8643 = ORIENTED_EDGE('',*,*,#6822,.F.) ;
#8644 = ORIENTED_EDGE('',*,*,#6807,.F.) ;
#8645 = ORIENTED_EDGE('',*,*,#6823,.F.) ;
#8646 = ORIENTED_EDGE('',*,*,#6824,.T.) ;
#8647 = ORIENTED_EDGE('',*,*,#6825,.F.) ;
#8648 = ORIENTED_EDGE('',*,*,#6824,.F.) ;
#8649 = ORIENTED_EDGE('',*,*,#6826,.F.) ;
#8650 = ORIENTED_EDGE('',*,*,#6825,.T.) ;
#8651 = ORIENTED_EDGE('',*,*,#6820,.T.) ;
#8652 = ORIENTED_EDGE('',*,*,#6785,.T.) ;
#8653 = ORIENTED_EDGE('',*,*,#6805,.T.) ;
#8654 = ORIENTED_EDGE('',*,*,#6810,.T.) ;
#8655 = ORIENTED_EDGE('',*,*,#6826,.T.) ;
#8656 = ORIENTED_EDGE('',*,*,#6823,.T.) ;
#8657 = ORIENTED_EDGE('',*,*,#6806,.T.) ;
#8658 = ORIENTED_EDGE('',*,*,#6802,.T.) ;
#8659 = ORIENTED_EDGE('',*,*,#6790,.T.) ;
#8660 = ORIENTED_EDGE('',*,*,#6766,.T.) ;
#8661 = ORIENTED_EDGE('',*,*,#6769,.T.) ;
#8662 = ORIENTED_EDGE('',*,*,#6772,.T.) ;
#8663 = ORIENTED_EDGE('',*,*,#6775,.T.) ;
#8664 = ORIENTED_EDGE('',*,*,#6778,.T.) ;
#8665 = ORIENTED_EDGE('',*,*,#6781,.T.) ;
#8666 = ORIENTED_EDGE('',*,*,#6827,.T.) ;
#8667 = ORIENTED_EDGE('',*,*,#6828,.F.) ;
#8668 = ORIENTED_EDGE('',*,*,#6829,.T.) ;
#8669 = ORIENTED_EDGE('',*,*,#6830,.F.) ;
#8670 = ORIENTED_EDGE('',*,*,#6829,.F.) ;
#8671 = ORIENTED_EDGE('',*,*,#6831,.T.) ;
#8672 = ORIENTED_EDGE('',*,*,#6832,.T.) ;
#8673 = ORIENTED_EDGE('',*,*,#6833,.F.) ;
#8674 = ORIENTED_EDGE('',*,*,#6832,.F.) ;
#8675 = ORIENTED_EDGE('',*,*,#6831,.F.) ;
#8676 = ORIENTED_EDGE('',*,*,#6830,.T.) ;
#8677 = ORIENTED_EDGE('',*,*,#6834,.F.) ;
#8678 = ORIENTED_EDGE('',*,*,#6835,.T.) ;
#8679 = ORIENTED_EDGE('',*,*,#6836,.T.) ;
#8680 = ORIENTED_EDGE('',*,*,#6835,.F.) ;
#8681 = ORIENTED_EDGE('',*,*,#6836,.F.) ;
#8682 = ORIENTED_EDGE('',*,*,#6828,.T.) ;
#8683 = ORIENTED_EDGE('',*,*,#6837,.F.) ;
#8684 = ORIENTED_EDGE('',*,*,#6838,.T.) ;
#8685 = ORIENTED_EDGE('',*,*,#6765,.F.) ;
#8686 = ORIENTED_EDGE('',*,*,#6838,.F.) ;
#8687 = ORIENTED_EDGE('',*,*,#6837,.T.) ;
#8688 = ORIENTED_EDGE('',*,*,#6833,.T.) ;
#8689 = ORIENTED_EDGE('',*,*,#6827,.F.) ;
#8690 = ORIENTED_EDGE('',*,*,#6839,.T.) ;
#8691 = ORIENTED_EDGE('',*,*,#6840,.F.) ;
#8692 = ORIENTED_EDGE('',*,*,#6839,.F.) ;
#8693 = ORIENTED_EDGE('',*,*,#6840,.T.) ;
#8694 = ORIENTED_EDGE('',*,*,#6834,.T.) ;
#8695 = ORIENTED_EDGE('',*,*,#6803,.T.) ;
#8696 = ORIENTED_EDGE('',*,*,#6768,.T.) ;
#8697 = ORIENTED_EDGE('',*,*,#6771,.T.) ;
#8698 = ORIENTED_EDGE('',*,*,#6774,.T.) ;
#8699 = ORIENTED_EDGE('',*,*,#6777,.T.) ;
#8700 = ORIENTED_EDGE('',*,*,#6780,.T.) ;
#8701 = ORIENTED_EDGE('',*,*,#6783,.T.) ;
#8702 = ORIENTED_EDGE('',*,*,#6747,.T.) ;
#8703 = ORIENTED_EDGE('',*,*,#6841,.F.) ;
#8704 = ORIENTED_EDGE('',*,*,#6842,.T.) ;
#8705 = ORIENTED_EDGE('',*,*,#6843,.F.) ;
#8706 = ORIENTED_EDGE('',*,*,#6842,.F.) ;
#8707 = ORIENTED_EDGE('',*,*,#6844,.F.) ;
#8708 = ORIENTED_EDGE('',*,*,#6845,.T.) ;
#8709 = ORIENTED_EDGE('',*,*,#6846,.F.) ;
#8710 = ORIENTED_EDGE('',*,*,#6845,.F.) ;
#8711 = ORIENTED_EDGE('',*,*,#6847,.F.) ;
#8712 = ORIENTED_EDGE('',*,*,#6848,.T.) ;
#8713 = ORIENTED_EDGE('',*,*,#6849,.F.) ;
#8714 = ORIENTED_EDGE('',*,*,#6848,.F.) ;
#8715 = ORIENTED_EDGE('',*,*,#6850,.F.) ;
#8716 = ORIENTED_EDGE('',*,*,#6851,.T.) ;
#8717 = ORIENTED_EDGE('',*,*,#6852,.F.) ;
#8718 = ORIENTED_EDGE('',*,*,#6851,.F.) ;
#8719 = ORIENTED_EDGE('',*,*,#6853,.F.) ;
#8720 = ORIENTED_EDGE('',*,*,#6854,.T.) ;
#8721 = ORIENTED_EDGE('',*,*,#6855,.F.) ;
#8722 = ORIENTED_EDGE('',*,*,#6854,.F.) ;
#8723 = ORIENTED_EDGE('',*,*,#6856,.F.) ;
#8724 = ORIENTED_EDGE('',*,*,#6857,.T.) ;
#8725 = ORIENTED_EDGE('',*,*,#6858,.F.) ;
#8726 = ORIENTED_EDGE('',*,*,#6857,.F.) ;
#8727 = ORIENTED_EDGE('',*,*,#6859,.F.) ;
#8728 = ORIENTED_EDGE('',*,*,#6860,.T.) ;
#8729 = ORIENTED_EDGE('',*,*,#6861,.F.) ;
#8730 = ORIENTED_EDGE('',*,*,#6860,.F.) ;
#8731 = ORIENTED_EDGE('',*,*,#6862,.F.) ;
#8732 = ORIENTED_EDGE('',*,*,#6863,.T.) ;
#8733 = ORIENTED_EDGE('',*,*,#6864,.F.) ;
#8734 = ORIENTED_EDGE('',*,*,#6863,.F.) ;
#8735 = ORIENTED_EDGE('',*,*,#6865,.F.) ;
#8736 = ORIENTED_EDGE('',*,*,#6866,.T.) ;
#8737 = ORIENTED_EDGE('',*,*,#6867,.F.) ;
#8738 = ORIENTED_EDGE('',*,*,#6866,.F.) ;
#8739 = ORIENTED_EDGE('',*,*,#6865,.T.) ;
#8740 = ORIENTED_EDGE('',*,*,#6864,.T.) ;
#8741 = ORIENTED_EDGE('',*,*,#6868,.F.) ;
#8742 = ORIENTED_EDGE('',*,*,#6869,.T.) ;
#8743 = ORIENTED_EDGE('',*,*,#6870,.F.) ;
#8744 = ORIENTED_EDGE('',*,*,#6869,.F.) ;
#8745 = ORIENTED_EDGE('',*,*,#6871,.F.) ;
#8746 = ORIENTED_EDGE('',*,*,#6872,.T.) ;
#8747 = ORIENTED_EDGE('',*,*,#6873,.F.) ;
#8748 = ORIENTED_EDGE('',*,*,#6872,.F.) ;
#8749 = ORIENTED_EDGE('',*,*,#6871,.T.) ;
#8750 = ORIENTED_EDGE('',*,*,#6870,.T.) ;
#8751 = ORIENTED_EDGE('',*,*,#6874,.T.) ;
#8752 = ORIENTED_EDGE('',*,*,#6875,.T.) ;
#8753 = ORIENTED_EDGE('',*,*,#6876,.F.) ;
#8754 = ORIENTED_EDGE('',*,*,#6875,.F.) ;
#8755 = ORIENTED_EDGE('',*,*,#6874,.F.) ;
#8756 = ORIENTED_EDGE('',*,*,#6877,.F.) ;
#8757 = ORIENTED_EDGE('',*,*,#6878,.F.) ;
#8758 = ORIENTED_EDGE('',*,*,#6879,.T.) ;
#8759 = ORIENTED_EDGE('',*,*,#6877,.T.) ;
#8760 = ORIENTED_EDGE('',*,*,#6879,.F.) ;
#8761 = ORIENTED_EDGE('',*,*,#6880,.F.) ;
#8762 = ORIENTED_EDGE('',*,*,#6881,.T.) ;
#8763 = ORIENTED_EDGE('',*,*,#6882,.T.) ;
#8764 = ORIENTED_EDGE('',*,*,#6881,.F.) ;
#8765 = ORIENTED_EDGE('',*,*,#6882,.F.) ;
#8766 = ORIENTED_EDGE('',*,*,#6841,.T.) ;
#8767 = ORIENTED_EDGE('',*,*,#6862,.T.) ;
#8768 = ORIENTED_EDGE('',*,*,#6868,.T.) ;
#8769 = ORIENTED_EDGE('',*,*,#6878,.T.) ;
#8770 = ORIENTED_EDGE('',*,*,#6883,.F.) ;
#8771 = ORIENTED_EDGE('',*,*,#6884,.T.) ;
#8772 = ORIENTED_EDGE('',*,*,#6885,.F.) ;
#8773 = ORIENTED_EDGE('',*,*,#6884,.F.) ;
#8774 = ORIENTED_EDGE('',*,*,#6885,.T.) ;
#8775 = ORIENTED_EDGE('',*,*,#6844,.T.) ;
#8776 = ORIENTED_EDGE('',*,*,#6847,.T.) ;
#8777 = ORIENTED_EDGE('',*,*,#6850,.T.) ;
#8778 = ORIENTED_EDGE('',*,*,#6853,.T.) ;
#8779 = ORIENTED_EDGE('',*,*,#6856,.T.) ;
#8780 = ORIENTED_EDGE('',*,*,#6859,.T.) ;
#8781 = ORIENTED_EDGE('',*,*,#6880,.T.) ;
#8782 = ORIENTED_EDGE('',*,*,#6883,.T.) ;
#8783 = ORIENTED_EDGE('',*,*,#6846,.T.) ;
#8784 = ORIENTED_EDGE('',*,*,#6876,.T.) ;
#8785 = ORIENTED_EDGE('',*,*,#6873,.T.) ;
#8786 = ORIENTED_EDGE('',*,*,#6867,.T.) ;
#8787 = ORIENTED_EDGE('',*,*,#6861,.T.) ;
#8788 = ORIENTED_EDGE('',*,*,#6858,.T.) ;
#8789 = ORIENTED_EDGE('',*,*,#6855,.T.) ;
#8790 = ORIENTED_EDGE('',*,*,#6852,.T.) ;
#8791 = ORIENTED_EDGE('',*,*,#6849,.T.) ;
#8792 = ORIENTED_EDGE('',*,*,#6843,.T.) ;
#8793 = ORIENTED_EDGE('',*,*,#6886,.F.) ;
#8794 = ORIENTED_EDGE('',*,*,#6887,.T.) ;
#8795 = ORIENTED_EDGE('',*,*,#6888,.F.) ;
#8796 = ORIENTED_EDGE('',*,*,#6887,.F.) ;
#8797 = ORIENTED_EDGE('',*,*,#6888,.T.) ;
#8798 = ORIENTED_EDGE('',*,*,#6886,.T.) ;
#8799 = ORIENTED_EDGE('',*,*,#6889,.F.) ;
#8800 = ORIENTED_EDGE('',*,*,#6890,.T.) ;
#8801 = ORIENTED_EDGE('',*,*,#6891,.F.) ;
#8802 = ORIENTED_EDGE('',*,*,#6890,.F.) ;
#8803 = ORIENTED_EDGE('',*,*,#6892,.F.) ;
#8804 = ORIENTED_EDGE('',*,*,#6893,.T.) ;
#8805 = ORIENTED_EDGE('',*,*,#6894,.F.) ;
#8806 = ORIENTED_EDGE('',*,*,#6893,.F.) ;
#8807 = ORIENTED_EDGE('',*,*,#6895,.F.) ;
#8808 = ORIENTED_EDGE('',*,*,#6896,.T.) ;
#8809 = ORIENTED_EDGE('',*,*,#6897,.F.) ;
#8810 = ORIENTED_EDGE('',*,*,#6896,.F.) ;
#8811 = ORIENTED_EDGE('',*,*,#6898,.F.) ;
#8812 = ORIENTED_EDGE('',*,*,#6899,.T.) ;
#8813 = ORIENTED_EDGE('',*,*,#6900,.F.) ;
#8814 = ORIENTED_EDGE('',*,*,#6899,.F.) ;
#8815 = ORIENTED_EDGE('',*,*,#6901,.F.) ;
#8816 = ORIENTED_EDGE('',*,*,#6902,.T.) ;
#8817 = ORIENTED_EDGE('',*,*,#6903,.F.) ;
#8818 = ORIENTED_EDGE('',*,*,#6902,.F.) ;
#8819 = ORIENTED_EDGE('',*,*,#6904,.F.) ;
#8820 = ORIENTED_EDGE('',*,*,#6905,.T.) ;
#8821 = ORIENTED_EDGE('',*,*,#6906,.F.) ;
#8822 = ORIENTED_EDGE('',*,*,#6905,.F.) ;
#8823 = ORIENTED_EDGE('',*,*,#6907,.F.) ;
#8824 = ORIENTED_EDGE('',*,*,#6908,.T.) ;
#8825 = ORIENTED_EDGE('',*,*,#6909,.F.) ;
#8826 = ORIENTED_EDGE('',*,*,#6908,.F.) ;
#8827 = ORIENTED_EDGE('',*,*,#6910,.F.) ;
#8828 = ORIENTED_EDGE('',*,*,#6911,.T.) ;
#8829 = ORIENTED_EDGE('',*,*,#6912,.F.) ;
#8830 = ORIENTED_EDGE('',*,*,#6911,.F.) ;
#8831 = ORIENTED_EDGE('',*,*,#6912,.T.) ;
#8832 = ORIENTED_EDGE('',*,*,#6889,.T.) ;
#8833 = ORIENTED_EDGE('',*,*,#6892,.T.) ;
#8834 = ORIENTED_EDGE('',*,*,#6895,.T.) ;
#8835 = ORIENTED_EDGE('',*,*,#6898,.T.) ;
#8836 = ORIENTED_EDGE('',*,*,#6901,.T.) ;
#8837 = ORIENTED_EDGE('',*,*,#6904,.T.) ;
#8838 = ORIENTED_EDGE('',*,*,#6907,.T.) ;
#8839 = ORIENTED_EDGE('',*,*,#6910,.T.) ;
#8840 = ORIENTED_EDGE('',*,*,#6891,.T.) ;
#8841 = ORIENTED_EDGE('',*,*,#6894,.T.) ;
#8842 = ORIENTED_EDGE('',*,*,#6897,.T.) ;
#8843 = ORIENTED_EDGE('',*,*,#6900,.T.) ;
#8844 = ORIENTED_EDGE('',*,*,#6903,.T.) ;
#8845 = ORIENTED_EDGE('',*,*,#6906,.T.) ;
#8846 = ORIENTED_EDGE('',*,*,#6909,.T.) ;
#8847 = ORIENTED_EDGE('',*,*,#6913,.F.) ;
#8848 = ORIENTED_EDGE('',*,*,#6914,.F.) ;
#8849 = ORIENTED_EDGE('',*,*,#6915,.F.) ;
#8850 = ORIENTED_EDGE('',*,*,#6916,.F.) ;
#8851 = ORIENTED_EDGE('',*,*,#6917,.F.) ;
#8852 = ORIENTED_EDGE('',*,*,#6915,.T.) ;
#8853 = ORIENTED_EDGE('',*,*,#6918,.T.) ;
#8854 = ORIENTED_EDGE('',*,*,#6919,.T.) ;
#8855 = ORIENTED_EDGE('',*,*,#6920,.F.) ;
#8856 = ORIENTED_EDGE('',*,*,#6921,.F.) ;
#8857 = ORIENTED_EDGE('',*,*,#6919,.F.) ;
#8858 = ORIENTED_EDGE('',*,*,#6922,.F.) ;
#8859 = ORIENTED_EDGE('',*,*,#6923,.F.) ;
#8860 = ORIENTED_EDGE('',*,*,#6922,.T.) ;
#8861 = ORIENTED_EDGE('',*,*,#6918,.F.) ;
#8862 = ORIENTED_EDGE('',*,*,#6914,.T.) ;
#8863 = ORIENTED_EDGE('',*,*,#6924,.T.) ;
#8864 = ORIENTED_EDGE('',*,*,#6925,.T.) ;
#8865 = ORIENTED_EDGE('',*,*,#6926,.F.) ;
#8866 = ORIENTED_EDGE('',*,*,#6916,.T.) ;
#8867 = ORIENTED_EDGE('',*,*,#6917,.T.) ;
#8868 = ORIENTED_EDGE('',*,*,#6921,.T.) ;
#8869 = ORIENTED_EDGE('',*,*,#6927,.F.) ;
#8870 = ORIENTED_EDGE('',*,*,#6925,.F.) ;
#8871 = ORIENTED_EDGE('',*,*,#6928,.T.) ;
#8872 = ORIENTED_EDGE('',*,*,#6929,.T.) ;
#8873 = ORIENTED_EDGE('',*,*,#6930,.T.) ;
#8874 = ORIENTED_EDGE('',*,*,#6929,.F.) ;
#8875 = ORIENTED_EDGE('',*,*,#6924,.F.) ;
#8876 = ORIENTED_EDGE('',*,*,#6930,.F.) ;
#8877 = ORIENTED_EDGE('',*,*,#6931,.F.) ;
#8878 = ORIENTED_EDGE('',*,*,#6928,.F.) ;
#8879 = ORIENTED_EDGE('',*,*,#6932,.T.) ;
#8880 = ORIENTED_EDGE('',*,*,#6933,.T.) ;
#8881 = ORIENTED_EDGE('',*,*,#6931,.T.) ;
#8882 = ORIENTED_EDGE('',*,*,#6933,.F.) ;
#8883 = ORIENTED_EDGE('',*,*,#6934,.F.) ;
#8884 = ORIENTED_EDGE('',*,*,#6935,.T.) ;
#8885 = ORIENTED_EDGE('',*,*,#6936,.F.) ;
#8886 = ORIENTED_EDGE('',*,*,#6935,.F.) ;
#8887 = ORIENTED_EDGE('',*,*,#6937,.F.) ;
#8888 = ORIENTED_EDGE('',*,*,#6938,.T.) ;
#8889 = ORIENTED_EDGE('',*,*,#6939,.F.) ;
#8890 = ORIENTED_EDGE('',*,*,#6938,.F.) ;
#8891 = ORIENTED_EDGE('',*,*,#6940,.F.) ;
#8892 = ORIENTED_EDGE('',*,*,#6941,.T.) ;
#8893 = ORIENTED_EDGE('',*,*,#6942,.F.) ;
#8894 = ORIENTED_EDGE('',*,*,#6941,.F.) ;
#8895 = ORIENTED_EDGE('',*,*,#6943,.T.) ;
#8896 = ORIENTED_EDGE('',*,*,#6934,.T.) ;
#8897 = ORIENTED_EDGE('',*,*,#6937,.T.) ;
#8898 = ORIENTED_EDGE('',*,*,#6940,.T.) ;
#8899 = ORIENTED_EDGE('',*,*,#6932,.F.) ;
#8900 = ORIENTED_EDGE('',*,*,#6944,.F.) ;
#8901 = ORIENTED_EDGE('',*,*,#6945,.T.) ;
#8902 = ORIENTED_EDGE('',*,*,#6943,.F.) ;
#8903 = ORIENTED_EDGE('',*,*,#6945,.F.) ;
#8904 = ORIENTED_EDGE('',*,*,#6946,.F.) ;
#8905 = ORIENTED_EDGE('',*,*,#6947,.T.) ;
#8906 = ORIENTED_EDGE('',*,*,#6948,.F.) ;
#8907 = ORIENTED_EDGE('',*,*,#6947,.F.) ;
#8908 = ORIENTED_EDGE('',*,*,#6946,.T.) ;
#8909 = ORIENTED_EDGE('',*,*,#6913,.T.) ;
#8910 = ORIENTED_EDGE('',*,*,#6926,.T.) ;
#8911 = ORIENTED_EDGE('',*,*,#6927,.T.) ;
#8912 = ORIENTED_EDGE('',*,*,#6920,.T.) ;
#8913 = ORIENTED_EDGE('',*,*,#6923,.T.) ;
#8914 = ORIENTED_EDGE('',*,*,#6944,.T.) ;
#8915 = ORIENTED_EDGE('',*,*,#6936,.T.) ;
#8916 = ORIENTED_EDGE('',*,*,#6939,.T.) ;
#8917 = ORIENTED_EDGE('',*,*,#6942,.T.) ;
#8918 = ORIENTED_EDGE('',*,*,#6948,.T.) ;
#8919 = ORIENTED_EDGE('',*,*,#6949,.F.) ;
#8920 = ORIENTED_EDGE('',*,*,#6950,.T.) ;
#8921 = ORIENTED_EDGE('',*,*,#6951,.T.) ;
#8922 = ORIENTED_EDGE('',*,*,#6950,.F.) ;
#8923 = ORIENTED_EDGE('',*,*,#6951,.F.) ;
#8924 = ORIENTED_EDGE('',*,*,#6952,.F.) ;
#8925 = ORIENTED_EDGE('',*,*,#6953,.T.) ;
#8926 = ORIENTED_EDGE('',*,*,#6954,.T.) ;
#8927 = ORIENTED_EDGE('',*,*,#6953,.F.) ;
#8928 = ORIENTED_EDGE('',*,*,#6954,.F.) ;
#8929 = ORIENTED_EDGE('',*,*,#6955,.F.) ;
#8930 = ORIENTED_EDGE('',*,*,#6956,.T.) ;
#8931 = ORIENTED_EDGE('',*,*,#6957,.T.) ;
#8932 = ORIENTED_EDGE('',*,*,#6956,.F.) ;
#8933 = ORIENTED_EDGE('',*,*,#6957,.F.) ;
#8934 = ORIENTED_EDGE('',*,*,#6958,.F.) ;
#8935 = ORIENTED_EDGE('',*,*,#6959,.T.) ;
#8936 = ORIENTED_EDGE('',*,*,#6960,.T.) ;
#8937 = ORIENTED_EDGE('',*,*,#6959,.F.) ;
#8938 = ORIENTED_EDGE('',*,*,#6960,.F.) ;
#8939 = ORIENTED_EDGE('',*,*,#6961,.F.) ;
#8940 = ORIENTED_EDGE('',*,*,#6962,.T.) ;
#8941 = ORIENTED_EDGE('',*,*,#6963,.T.) ;
#8942 = ORIENTED_EDGE('',*,*,#6962,.F.) ;
#8943 = ORIENTED_EDGE('',*,*,#6963,.F.) ;
#8944 = ORIENTED_EDGE('',*,*,#6964,.F.) ;
#8945 = ORIENTED_EDGE('',*,*,#6965,.T.) ;
#8946 = ORIENTED_EDGE('',*,*,#6966,.T.) ;
#8947 = ORIENTED_EDGE('',*,*,#6965,.F.) ;
#8948 = ORIENTED_EDGE('',*,*,#6966,.F.) ;
#8949 = ORIENTED_EDGE('',*,*,#6967,.F.) ;
#8950 = ORIENTED_EDGE('',*,*,#6968,.T.) ;
#8951 = ORIENTED_EDGE('',*,*,#6969,.T.) ;
#8952 = ORIENTED_EDGE('',*,*,#6968,.F.) ;
#8953 = ORIENTED_EDGE('',*,*,#6969,.F.) ;
#8954 = ORIENTED_EDGE('',*,*,#6970,.F.) ;
#8955 = ORIENTED_EDGE('',*,*,#6971,.T.) ;
#8956 = ORIENTED_EDGE('',*,*,#6972,.T.) ;
#8957 = ORIENTED_EDGE('',*,*,#6971,.F.) ;
#8958 = ORIENTED_EDGE('',*,*,#6972,.F.) ;
#8959 = ORIENTED_EDGE('',*,*,#6973,.F.) ;
#8960 = ORIENTED_EDGE('',*,*,#6974,.T.) ;
#8961 = ORIENTED_EDGE('',*,*,#6975,.T.) ;
#8962 = ORIENTED_EDGE('',*,*,#6974,.F.) ;
#8963 = ORIENTED_EDGE('',*,*,#6975,.F.) ;
#8964 = ORIENTED_EDGE('',*,*,#6976,.F.) ;
#8965 = ORIENTED_EDGE('',*,*,#6977,.T.) ;
#8966 = ORIENTED_EDGE('',*,*,#6978,.T.) ;
#8967 = ORIENTED_EDGE('',*,*,#6977,.F.) ;
#8968 = ORIENTED_EDGE('',*,*,#6978,.F.) ;
#8969 = ORIENTED_EDGE('',*,*,#6979,.F.) ;
#8970 = ORIENTED_EDGE('',*,*,#6980,.T.) ;
#8971 = ORIENTED_EDGE('',*,*,#6981,.T.) ;
#8972 = ORIENTED_EDGE('',*,*,#6980,.F.) ;
#8973 = ORIENTED_EDGE('',*,*,#6981,.F.) ;
#8974 = ORIENTED_EDGE('',*,*,#6982,.F.) ;
#8975 = ORIENTED_EDGE('',*,*,#6983,.T.) ;
#8976 = ORIENTED_EDGE('',*,*,#6984,.T.) ;
#8977 = ORIENTED_EDGE('',*,*,#6983,.F.) ;
#8978 = ORIENTED_EDGE('',*,*,#6984,.F.) ;
#8979 = ORIENTED_EDGE('',*,*,#6985,.F.) ;
#8980 = ORIENTED_EDGE('',*,*,#6986,.T.) ;
#8981 = ORIENTED_EDGE('',*,*,#6987,.T.) ;
#8982 = ORIENTED_EDGE('',*,*,#6986,.F.) ;
#8983 = ORIENTED_EDGE('',*,*,#6987,.F.) ;
#8984 = ORIENTED_EDGE('',*,*,#6988,.F.) ;
#8985 = ORIENTED_EDGE('',*,*,#6989,.T.) ;
#8986 = ORIENTED_EDGE('',*,*,#6990,.T.) ;
#8987 = ORIENTED_EDGE('',*,*,#6989,.F.) ;
#8988 = ORIENTED_EDGE('',*,*,#6990,.F.) ;
#8989 = ORIENTED_EDGE('',*,*,#6991,.F.) ;
#8990 = ORIENTED_EDGE('',*,*,#6992,.T.) ;
#8991 = ORIENTED_EDGE('',*,*,#6993,.T.) ;
#8992 = ORIENTED_EDGE('',*,*,#6992,.F.) ;
#8993 = ORIENTED_EDGE('',*,*,#6993,.F.) ;
#8994 = ORIENTED_EDGE('',*,*,#6994,.F.) ;
#8995 = ORIENTED_EDGE('',*,*,#6995,.T.) ;
#8996 = ORIENTED_EDGE('',*,*,#6996,.T.) ;
#8997 = ORIENTED_EDGE('',*,*,#6995,.F.) ;
#8998 = ORIENTED_EDGE('',*,*,#6996,.F.) ;
#8999 = ORIENTED_EDGE('',*,*,#6997,.F.) ;
#9000 = ORIENTED_EDGE('',*,*,#6998,.T.) ;
#9001 = ORIENTED_EDGE('',*,*,#6999,.T.) ;
#9002 = ORIENTED_EDGE('',*,*,#6998,.F.) ;
#9003 = ORIENTED_EDGE('',*,*,#6999,.F.) ;
#9004 = ORIENTED_EDGE('',*,*,#7000,.F.) ;
#9005 = ORIENTED_EDGE('',*,*,#7001,.T.) ;
#9006 = ORIENTED_EDGE('',*,*,#7002,.T.) ;
#9007 = ORIENTED_EDGE('',*,*,#7001,.F.) ;
#9008 = ORIENTED_EDGE('',*,*,#7002,.F.) ;
#9009 = ORIENTED_EDGE('',*,*,#7003,.F.) ;
#9010 = ORIENTED_EDGE('',*,*,#7004,.T.) ;
#9011 = ORIENTED_EDGE('',*,*,#7005,.T.) ;
#9012 = ORIENTED_EDGE('',*,*,#7004,.F.) ;
#9013 = ORIENTED_EDGE('',*,*,#7005,.F.) ;
#9014 = ORIENTED_EDGE('',*,*,#7006,.F.) ;
#9015 = ORIENTED_EDGE('',*,*,#7007,.T.) ;
#9016 = ORIENTED_EDGE('',*,*,#7008,.T.) ;
#9017 = ORIENTED_EDGE('',*,*,#7007,.F.) ;
#9018 = ORIENTED_EDGE('',*,*,#7008,.F.) ;
#9019 = ORIENTED_EDGE('',*,*,#7009,.F.) ;
#9020 = ORIENTED_EDGE('',*,*,#7010,.T.) ;
#9021 = ORIENTED_EDGE('',*,*,#7011,.T.) ;
#9022 = ORIENTED_EDGE('',*,*,#7010,.F.) ;
#9023 = ORIENTED_EDGE('',*,*,#7011,.F.) ;
#9024 = ORIENTED_EDGE('',*,*,#7012,.F.) ;
#9025 = ORIENTED_EDGE('',*,*,#7013,.T.) ;
#9026 = ORIENTED_EDGE('',*,*,#7014,.T.) ;
#9027 = ORIENTED_EDGE('',*,*,#7013,.F.) ;
#9028 = ORIENTED_EDGE('',*,*,#7014,.F.) ;
#9029 = ORIENTED_EDGE('',*,*,#7015,.F.) ;
#9030 = ORIENTED_EDGE('',*,*,#7016,.T.) ;
#9031 = ORIENTED_EDGE('',*,*,#7017,.T.) ;
#9032 = ORIENTED_EDGE('',*,*,#7016,.F.) ;
#9033 = ORIENTED_EDGE('',*,*,#7017,.F.) ;
#9034 = ORIENTED_EDGE('',*,*,#7018,.F.) ;
#9035 = ORIENTED_EDGE('',*,*,#7019,.T.) ;
#9036 = ORIENTED_EDGE('',*,*,#7020,.T.) ;
#9037 = ORIENTED_EDGE('',*,*,#7019,.F.) ;
#9038 = ORIENTED_EDGE('',*,*,#7020,.F.) ;
#9039 = ORIENTED_EDGE('',*,*,#7021,.F.) ;
#9040 = ORIENTED_EDGE('',*,*,#7022,.T.) ;
#9041 = ORIENTED_EDGE('',*,*,#7023,.F.) ;
#9042 = ORIENTED_EDGE('',*,*,#7022,.F.) ;
#9043 = ORIENTED_EDGE('',*,*,#7024,.F.) ;
#9044 = ORIENTED_EDGE('',*,*,#7025,.T.) ;
#9045 = ORIENTED_EDGE('',*,*,#7026,.F.) ;
#9046 = ORIENTED_EDGE('',*,*,#7025,.F.) ;
#9047 = ORIENTED_EDGE('',*,*,#7027,.F.) ;
#9048 = ORIENTED_EDGE('',*,*,#7028,.T.) ;
#9049 = ORIENTED_EDGE('',*,*,#7029,.F.) ;
#9050 = ORIENTED_EDGE('',*,*,#7028,.F.) ;
#9051 = ORIENTED_EDGE('',*,*,#7030,.F.) ;
#9052 = ORIENTED_EDGE('',*,*,#7031,.T.) ;
#9053 = ORIENTED_EDGE('',*,*,#7032,.F.) ;
#9054 = ORIENTED_EDGE('',*,*,#7031,.F.) ;
#9055 = ORIENTED_EDGE('',*,*,#7033,.F.) ;
#9056 = ORIENTED_EDGE('',*,*,#7034,.T.) ;
#9057 = ORIENTED_EDGE('',*,*,#7035,.F.) ;
#9058 = ORIENTED_EDGE('',*,*,#7034,.F.) ;
#9059 = ORIENTED_EDGE('',*,*,#7036,.F.) ;
#9060 = ORIENTED_EDGE('',*,*,#7037,.T.) ;
#9061 = ORIENTED_EDGE('',*,*,#7038,.F.) ;
#9062 = ORIENTED_EDGE('',*,*,#7037,.F.) ;
#9063 = ORIENTED_EDGE('',*,*,#7039,.F.) ;
#9064 = ORIENTED_EDGE('',*,*,#7040,.T.) ;
#9065 = ORIENTED_EDGE('',*,*,#7041,.F.) ;
#9066 = ORIENTED_EDGE('',*,*,#7040,.F.) ;
#9067 = ORIENTED_EDGE('',*,*,#7042,.F.) ;
#9068 = ORIENTED_EDGE('',*,*,#7043,.T.) ;
#9069 = ORIENTED_EDGE('',*,*,#7044,.F.) ;
#9070 = ORIENTED_EDGE('',*,*,#7043,.F.) ;
#9071 = ORIENTED_EDGE('',*,*,#7045,.F.) ;
#9072 = ORIENTED_EDGE('',*,*,#7046,.T.) ;
#9073 = ORIENTED_EDGE('',*,*,#7047,.F.) ;
#9074 = ORIENTED_EDGE('',*,*,#7046,.F.) ;
#9075 = ORIENTED_EDGE('',*,*,#7048,.F.) ;
#9076 = ORIENTED_EDGE('',*,*,#7049,.T.) ;
#9077 = ORIENTED_EDGE('',*,*,#7050,.F.) ;
#9078 = ORIENTED_EDGE('',*,*,#7049,.F.) ;
#9079 = ORIENTED_EDGE('',*,*,#7051,.F.) ;
#9080 = ORIENTED_EDGE('',*,*,#7052,.T.) ;
#9081 = ORIENTED_EDGE('',*,*,#7053,.F.) ;
#9082 = ORIENTED_EDGE('',*,*,#7052,.F.) ;
#9083 = ORIENTED_EDGE('',*,*,#7054,.F.) ;
#9084 = ORIENTED_EDGE('',*,*,#7055,.T.) ;
#9085 = ORIENTED_EDGE('',*,*,#7056,.F.) ;
#9086 = ORIENTED_EDGE('',*,*,#7055,.F.) ;
#9087 = ORIENTED_EDGE('',*,*,#7057,.F.) ;
#9088 = ORIENTED_EDGE('',*,*,#7058,.T.) ;
#9089 = ORIENTED_EDGE('',*,*,#7059,.F.) ;
#9090 = ORIENTED_EDGE('',*,*,#7058,.F.) ;
#9091 = ORIENTED_EDGE('',*,*,#7060,.F.) ;
#9092 = ORIENTED_EDGE('',*,*,#7061,.T.) ;
#9093 = ORIENTED_EDGE('',*,*,#7062,.F.) ;
#9094 = ORIENTED_EDGE('',*,*,#7061,.F.) ;
#9095 = ORIENTED_EDGE('',*,*,#7063,.F.) ;
#9096 = ORIENTED_EDGE('',*,*,#7064,.T.) ;
#9097 = ORIENTED_EDGE('',*,*,#7065,.F.) ;
#9098 = ORIENTED_EDGE('',*,*,#7064,.F.) ;
#9099 = ORIENTED_EDGE('',*,*,#7066,.F.) ;
#9100 = ORIENTED_EDGE('',*,*,#7067,.T.) ;
#9101 = ORIENTED_EDGE('',*,*,#7068,.F.) ;
#9102 = ORIENTED_EDGE('',*,*,#7067,.F.) ;
#9103 = ORIENTED_EDGE('',*,*,#7069,.F.) ;
#9104 = ORIENTED_EDGE('',*,*,#7070,.T.) ;
#9105 = ORIENTED_EDGE('',*,*,#7071,.F.) ;
#9106 = ORIENTED_EDGE('',*,*,#7070,.F.) ;
#9107 = ORIENTED_EDGE('',*,*,#7072,.F.) ;
#9108 = ORIENTED_EDGE('',*,*,#7073,.T.) ;
#9109 = ORIENTED_EDGE('',*,*,#7074,.F.) ;
#9110 = ORIENTED_EDGE('',*,*,#7073,.F.) ;
#9111 = ORIENTED_EDGE('',*,*,#7075,.F.) ;
#9112 = ORIENTED_EDGE('',*,*,#7076,.T.) ;
#9113 = ORIENTED_EDGE('',*,*,#7077,.F.) ;
#9114 = ORIENTED_EDGE('',*,*,#7076,.F.) ;
#9115 = ORIENTED_EDGE('',*,*,#7078,.F.) ;
#9116 = ORIENTED_EDGE('',*,*,#7079,.T.) ;
#9117 = ORIENTED_EDGE('',*,*,#7080,.F.) ;
#9118 = ORIENTED_EDGE('',*,*,#7079,.F.) ;
#9119 = ORIENTED_EDGE('',*,*,#7081,.F.) ;
#9120 = ORIENTED_EDGE('',*,*,#7082,.T.) ;
#9121 = ORIENTED_EDGE('',*,*,#7083,.F.) ;
#9122 = ORIENTED_EDGE('',*,*,#7082,.F.) ;
#9123 = ORIENTED_EDGE('',*,*,#7084,.F.) ;
#9124 = ORIENTED_EDGE('',*,*,#7085,.T.) ;
#9125 = ORIENTED_EDGE('',*,*,#7086,.F.) ;
#9126 = ORIENTED_EDGE('',*,*,#7085,.F.) ;
#9127 = ORIENTED_EDGE('',*,*,#7087,.F.) ;
#9128 = ORIENTED_EDGE('',*,*,#7088,.T.) ;
#9129 = ORIENTED_EDGE('',*,*,#7089,.F.) ;
#9130 = ORIENTED_EDGE('',*,*,#7088,.F.) ;
#9131 = ORIENTED_EDGE('',*,*,#7090,.F.) ;
#9132 = ORIENTED_EDGE('',*,*,#7091,.T.) ;
#9133 = ORIENTED_EDGE('',*,*,#7092,.F.) ;
#9134 = ORIENTED_EDGE('',*,*,#7091,.F.) ;
#9135 = ORIENTED_EDGE('',*,*,#7093,.F.) ;
#9136 = ORIENTED_EDGE('',*,*,#7094,.T.) ;
#9137 = ORIENTED_EDGE('',*,*,#7095,.F.) ;
#9138 = ORIENTED_EDGE('',*,*,#7094,.F.) ;
#9139 = ORIENTED_EDGE('',*,*,#7096,.F.) ;
#9140 = ORIENTED_EDGE('',*,*,#7097,.T.) ;
#9141 = ORIENTED_EDGE('',*,*,#7098,.F.) ;
#9142 = ORIENTED_EDGE('',*,*,#7097,.F.) ;
#9143 = ORIENTED_EDGE('',*,*,#7099,.F.) ;
#9144 = ORIENTED_EDGE('',*,*,#7100,.T.) ;
#9145 = ORIENTED_EDGE('',*,*,#7101,.F.) ;
#9146 = ORIENTED_EDGE('',*,*,#7100,.F.) ;
#9147 = ORIENTED_EDGE('',*,*,#7102,.F.) ;
#9148 = ORIENTED_EDGE('',*,*,#7103,.T.) ;
#9149 = ORIENTED_EDGE('',*,*,#7104,.F.) ;
#9150 = ORIENTED_EDGE('',*,*,#7103,.F.) ;
#9151 = ORIENTED_EDGE('',*,*,#7105,.F.) ;
#9152 = ORIENTED_EDGE('',*,*,#7106,.T.) ;
#9153 = ORIENTED_EDGE('',*,*,#7107,.F.) ;
#9154 = ORIENTED_EDGE('',*,*,#7106,.F.) ;
#9155 = ORIENTED_EDGE('',*,*,#7107,.T.) ;
#9156 = ORIENTED_EDGE('',*,*,#6952,.T.) ;
#9157 = ORIENTED_EDGE('',*,*,#6958,.T.) ;
#9158 = ORIENTED_EDGE('',*,*,#6964,.T.) ;
#9159 = ORIENTED_EDGE('',*,*,#6970,.T.) ;
#9160 = ORIENTED_EDGE('',*,*,#6976,.T.) ;
#9161 = ORIENTED_EDGE('',*,*,#6982,.T.) ;
#9162 = ORIENTED_EDGE('',*,*,#6988,.T.) ;
#9163 = ORIENTED_EDGE('',*,*,#6994,.T.) ;
#9164 = ORIENTED_EDGE('',*,*,#7000,.T.) ;
#9165 = ORIENTED_EDGE('',*,*,#7006,.T.) ;
#9166 = ORIENTED_EDGE('',*,*,#7012,.T.) ;
#9167 = ORIENTED_EDGE('',*,*,#7018,.T.) ;
#9168 = ORIENTED_EDGE('',*,*,#7024,.T.) ;
#9169 = ORIENTED_EDGE('',*,*,#7030,.T.) ;
#9170 = ORIENTED_EDGE('',*,*,#7036,.T.) ;
#9171 = ORIENTED_EDGE('',*,*,#7042,.T.) ;
#9172 = ORIENTED_EDGE('',*,*,#7048,.T.) ;
#9173 = ORIENTED_EDGE('',*,*,#7054,.T.) ;
#9174 = ORIENTED_EDGE('',*,*,#7060,.T.) ;
#9175 = ORIENTED_EDGE('',*,*,#7066,.T.) ;
#9176 = ORIENTED_EDGE('',*,*,#7072,.T.) ;
#9177 = ORIENTED_EDGE('',*,*,#7078,.T.) ;
#9178 = ORIENTED_EDGE('',*,*,#7102,.T.) ;
#9179 = ORIENTED_EDGE('',*,*,#7099,.T.) ;
#9180 = ORIENTED_EDGE('',*,*,#7096,.T.) ;
#9181 = ORIENTED_EDGE('',*,*,#7093,.T.) ;
#9182 = ORIENTED_EDGE('',*,*,#7090,.T.) ;
#9183 = ORIENTED_EDGE('',*,*,#7087,.T.) ;
#9184 = ORIENTED_EDGE('',*,*,#7084,.T.) ;
#9185 = ORIENTED_EDGE('',*,*,#7081,.T.) ;
#9186 = ORIENTED_EDGE('',*,*,#7075,.T.) ;
#9187 = ORIENTED_EDGE('',*,*,#7069,.T.) ;
#9188 = ORIENTED_EDGE('',*,*,#7063,.T.) ;
#9189 = ORIENTED_EDGE('',*,*,#7057,.T.) ;
#9190 = ORIENTED_EDGE('',*,*,#7051,.T.) ;
#9191 = ORIENTED_EDGE('',*,*,#7045,.T.) ;
#9192 = ORIENTED_EDGE('',*,*,#7039,.T.) ;
#9193 = ORIENTED_EDGE('',*,*,#7033,.T.) ;
#9194 = ORIENTED_EDGE('',*,*,#7027,.T.) ;
#9195 = ORIENTED_EDGE('',*,*,#7021,.T.) ;
#9196 = ORIENTED_EDGE('',*,*,#7015,.T.) ;
#9197 = ORIENTED_EDGE('',*,*,#7009,.T.) ;
#9198 = ORIENTED_EDGE('',*,*,#7003,.T.) ;
#9199 = ORIENTED_EDGE('',*,*,#6997,.T.) ;
#9200 = ORIENTED_EDGE('',*,*,#6991,.T.) ;
#9201 = ORIENTED_EDGE('',*,*,#6985,.T.) ;
#9202 = ORIENTED_EDGE('',*,*,#6979,.T.) ;
#9203 = ORIENTED_EDGE('',*,*,#6973,.T.) ;
#9204 = ORIENTED_EDGE('',*,*,#6967,.T.) ;
#9205 = ORIENTED_EDGE('',*,*,#6961,.T.) ;
#9206 = ORIENTED_EDGE('',*,*,#6955,.T.) ;
#9207 = ORIENTED_EDGE('',*,*,#6949,.T.) ;
#9208 = ORIENTED_EDGE('',*,*,#7105,.T.) ;
#9209 = ORIENTED_EDGE('',*,*,#7026,.T.) ;
#9210 = ORIENTED_EDGE('',*,*,#7032,.T.) ;
#9211 = ORIENTED_EDGE('',*,*,#7038,.T.) ;
#9212 = ORIENTED_EDGE('',*,*,#7044,.T.) ;
#9213 = ORIENTED_EDGE('',*,*,#7050,.T.) ;
#9214 = ORIENTED_EDGE('',*,*,#7056,.T.) ;
#9215 = ORIENTED_EDGE('',*,*,#7062,.T.) ;
#9216 = ORIENTED_EDGE('',*,*,#7068,.T.) ;
#9217 = ORIENTED_EDGE('',*,*,#7074,.T.) ;
#9218 = ORIENTED_EDGE('',*,*,#7080,.T.) ;
#9219 = ORIENTED_EDGE('',*,*,#7104,.T.) ;
#9220 = ORIENTED_EDGE('',*,*,#7101,.T.) ;
#9221 = ORIENTED_EDGE('',*,*,#7098,.T.) ;
#9222 = ORIENTED_EDGE('',*,*,#7095,.T.) ;
#9223 = ORIENTED_EDGE('',*,*,#7092,.T.) ;
#9224 = ORIENTED_EDGE('',*,*,#7089,.T.) ;
#9225 = ORIENTED_EDGE('',*,*,#7086,.T.) ;
#9226 = ORIENTED_EDGE('',*,*,#7083,.T.) ;
#9227 = ORIENTED_EDGE('',*,*,#7077,.T.) ;
#9228 = ORIENTED_EDGE('',*,*,#7071,.T.) ;
#9229 = ORIENTED_EDGE('',*,*,#7065,.T.) ;
#9230 = ORIENTED_EDGE('',*,*,#7059,.T.) ;
#9231 = ORIENTED_EDGE('',*,*,#7053,.T.) ;
#9232 = ORIENTED_EDGE('',*,*,#7047,.T.) ;
#9233 = ORIENTED_EDGE('',*,*,#7041,.T.) ;
#9234 = ORIENTED_EDGE('',*,*,#7035,.T.) ;
#9235 = ORIENTED_EDGE('',*,*,#7029,.T.) ;
#9236 = ORIENTED_EDGE('',*,*,#7023,.T.) ;
#9237 = ORIENTED_EDGE('',*,*,#7108,.F.) ;
#9238 = ORIENTED_EDGE('',*,*,#7109,.F.) ;
#9239 = ORIENTED_EDGE('',*,*,#7110,.F.) ;
#9240 = ORIENTED_EDGE('',*,*,#7111,.F.) ;
#9241 = ORIENTED_EDGE('',*,*,#7109,.T.) ;
#9242 = ORIENTED_EDGE('',*,*,#7112,.T.) ;
#9243 = ORIENTED_EDGE('',*,*,#7111,.T.) ;
#9244 = ORIENTED_EDGE('',*,*,#7112,.F.) ;
#9245 = ORIENTED_EDGE('',*,*,#7110,.T.) ;
#9246 = ORIENTED_EDGE('',*,*,#7113,.T.) ;
#9247 = ORIENTED_EDGE('',*,*,#7108,.T.) ;
#9248 = ORIENTED_EDGE('',*,*,#7113,.F.) ;
#9249 = ORIENTED_EDGE('',*,*,#7114,.T.) ;
#9250 = ORIENTED_EDGE('',*,*,#7115,.T.) ;
#9251 = ORIENTED_EDGE('',*,*,#7116,.F.) ;
#9252 = ORIENTED_EDGE('',*,*,#7117,.T.) ;
#9253 = ORIENTED_EDGE('',*,*,#7114,.F.) ;
#9254 = ORIENTED_EDGE('',*,*,#7117,.F.) ;
#9255 = ORIENTED_EDGE('',*,*,#7116,.T.) ;
#9256 = ORIENTED_EDGE('',*,*,#7118,.T.) ;
#9257 = ORIENTED_EDGE('',*,*,#7115,.F.) ;
#9258 = ORIENTED_EDGE('',*,*,#7119,.T.) ;
#9259 = ORIENTED_EDGE('',*,*,#7118,.F.) ;
#9260 = ORIENTED_EDGE('',*,*,#7119,.F.) ;
#9261 = ORIENTED_EDGE('',*,*,#7120,.F.) ;
#9262 = ORIENTED_EDGE('',*,*,#7121,.F.) ;
#9263 = ORIENTED_EDGE('',*,*,#7122,.F.) ;
#9264 = ORIENTED_EDGE('',*,*,#7123,.F.) ;
#9265 = ORIENTED_EDGE('',*,*,#7121,.T.) ;
#9266 = ORIENTED_EDGE('',*,*,#7124,.T.) ;
#9267 = ORIENTED_EDGE('',*,*,#7123,.T.) ;
#9268 = ORIENTED_EDGE('',*,*,#7124,.F.) ;
#9269 = ORIENTED_EDGE('',*,*,#7122,.T.) ;
#9270 = ORIENTED_EDGE('',*,*,#7125,.T.) ;
#9271 = ORIENTED_EDGE('',*,*,#7120,.T.) ;
#9272 = ORIENTED_EDGE('',*,*,#7125,.F.) ;
#9273 = ORIENTED_EDGE('',*,*,#7126,.T.) ;
#9274 = ORIENTED_EDGE('',*,*,#7127,.T.) ;
#9275 = ORIENTED_EDGE('',*,*,#7128,.F.) ;
#9276 = ORIENTED_EDGE('',*,*,#7129,.T.) ;
#9277 = ORIENTED_EDGE('',*,*,#7126,.F.) ;
#9278 = ORIENTED_EDGE('',*,*,#7129,.F.) ;
#9279 = ORIENTED_EDGE('',*,*,#7128,.T.) ;
#9280 = ORIENTED_EDGE('',*,*,#7130,.T.) ;
#9281 = ORIENTED_EDGE('',*,*,#7127,.F.) ;
#9282 = ORIENTED_EDGE('',*,*,#7131,.T.) ;
#9283 = ORIENTED_EDGE('',*,*,#7130,.F.) ;
#9284 = ORIENTED_EDGE('',*,*,#7131,.F.) ;
#9285 = ORIENTED_EDGE('',*,*,#7132,.F.) ;
#9286 = ORIENTED_EDGE('',*,*,#7133,.T.) ;
#9287 = ORIENTED_EDGE('',*,*,#7134,.F.) ;
#9288 = ORIENTED_EDGE('',*,*,#7133,.F.) ;
#9289 = ORIENTED_EDGE('',*,*,#7135,.F.) ;
#9290 = ORIENTED_EDGE('',*,*,#7136,.T.) ;
#9291 = ORIENTED_EDGE('',*,*,#7137,.F.) ;
#9292 = ORIENTED_EDGE('',*,*,#7136,.F.) ;
#9293 = ORIENTED_EDGE('',*,*,#7137,.T.) ;
#9294 = ORIENTED_EDGE('',*,*,#7132,.T.) ;
#9295 = ORIENTED_EDGE('',*,*,#7135,.T.) ;
#9296 = ORIENTED_EDGE('',*,*,#7134,.T.) ;
#9297 = ORIENTED_EDGE('',*,*,#7138,.F.) ;
#9298 = ORIENTED_EDGE('',*,*,#7139,.F.) ;
#9299 = ORIENTED_EDGE('',*,*,#7140,.F.) ;
#9300 = ORIENTED_EDGE('',*,*,#7141,.F.) ;
#9301 = ORIENTED_EDGE('',*,*,#7142,.F.) ;
#9302 = ORIENTED_EDGE('',*,*,#7143,.F.) ;
#9303 = ORIENTED_EDGE('',*,*,#7144,.F.) ;
#9304 = ORIENTED_EDGE('',*,*,#7145,.F.) ;
#9305 = ORIENTED_EDGE('',*,*,#7139,.T.) ;
#9306 = ORIENTED_EDGE('',*,*,#7146,.T.) ;
#9307 = ORIENTED_EDGE('',*,*,#7145,.T.) ;
#9308 = ORIENTED_EDGE('',*,*,#7147,.T.) ;
#9309 = ORIENTED_EDGE('',*,*,#7140,.T.) ;
#9310 = ORIENTED_EDGE('',*,*,#7147,.F.) ;
#9311 = ORIENTED_EDGE('',*,*,#7144,.T.) ;
#9312 = ORIENTED_EDGE('',*,*,#7148,.F.) ;
#9313 = ORIENTED_EDGE('',*,*,#7138,.T.) ;
#9314 = ORIENTED_EDGE('',*,*,#7149,.F.) ;
#9315 = ORIENTED_EDGE('',*,*,#7142,.T.) ;
#9316 = ORIENTED_EDGE('',*,*,#7146,.F.) ;
#9317 = ORIENTED_EDGE('',*,*,#7141,.T.) ;
#9318 = ORIENTED_EDGE('',*,*,#7148,.T.) ;
#9319 = ORIENTED_EDGE('',*,*,#7143,.T.) ;
#9320 = ORIENTED_EDGE('',*,*,#7149,.T.) ;
#9321 = ORIENTED_EDGE('',*,*,#7150,.F.) ;
#9322 = ORIENTED_EDGE('',*,*,#7151,.F.) ;
#9323 = ORIENTED_EDGE('',*,*,#7152,.F.) ;
#9324 = ORIENTED_EDGE('',*,*,#7153,.F.) ;
#9325 = ORIENTED_EDGE('',*,*,#7154,.F.) ;
#9326 = ORIENTED_EDGE('',*,*,#7155,.F.) ;
#9327 = ORIENTED_EDGE('',*,*,#7156,.F.) ;
#9328 = ORIENTED_EDGE('',*,*,#7157,.F.) ;
#9329 = ORIENTED_EDGE('',*,*,#7158,.F.) ;
#9330 = ORIENTED_EDGE('',*,*,#7157,.T.) ;
#9331 = ORIENTED_EDGE('',*,*,#7159,.F.) ;
#9332 = ORIENTED_EDGE('',*,*,#7151,.T.) ;
#9333 = ORIENTED_EDGE('',*,*,#7160,.T.) ;
#9334 = ORIENTED_EDGE('',*,*,#7152,.T.) ;
#9335 = ORIENTED_EDGE('',*,*,#7159,.T.) ;
#9336 = ORIENTED_EDGE('',*,*,#7156,.T.) ;
#9337 = ORIENTED_EDGE('',*,*,#7161,.T.) ;
#9338 = ORIENTED_EDGE('',*,*,#7153,.T.) ;
#9339 = ORIENTED_EDGE('',*,*,#7161,.F.) ;
#9340 = ORIENTED_EDGE('',*,*,#7155,.T.) ;
#9341 = ORIENTED_EDGE('',*,*,#7162,.F.) ;
#9342 = ORIENTED_EDGE('',*,*,#7163,.F.) ;
#9343 = ORIENTED_EDGE('',*,*,#7164,.T.) ;
#9344 = ORIENTED_EDGE('',*,*,#7165,.T.) ;
#9345 = ORIENTED_EDGE('',*,*,#7166,.T.) ;
#9346 = ORIENTED_EDGE('',*,*,#7167,.F.) ;
#9347 = ORIENTED_EDGE('',*,*,#7168,.T.) ;
#9348 = ORIENTED_EDGE('',*,*,#7169,.T.) ;
#9349 = ORIENTED_EDGE('',*,*,#7170,.T.) ;
#9350 = ORIENTED_EDGE('',*,*,#7171,.T.) ;
#9351 = ORIENTED_EDGE('',*,*,#7165,.F.) ;
#9352 = ORIENTED_EDGE('',*,*,#7172,.F.) ;
#9353 = ORIENTED_EDGE('',*,*,#7169,.F.) ;
#9354 = ORIENTED_EDGE('',*,*,#7163,.T.) ;
#9355 = ORIENTED_EDGE('',*,*,#7173,.F.) ;
#9356 = ORIENTED_EDGE('',*,*,#7174,.T.) ;
#9357 = ORIENTED_EDGE('',*,*,#7175,.F.) ;
#9358 = ORIENTED_EDGE('',*,*,#7167,.T.) ;
#9359 = ORIENTED_EDGE('',*,*,#7176,.F.) ;
#9360 = ORIENTED_EDGE('',*,*,#7177,.T.) ;
#9361 = ORIENTED_EDGE('',*,*,#7178,.F.) ;
#9362 = ORIENTED_EDGE('',*,*,#7175,.T.) ;
#9363 = ORIENTED_EDGE('',*,*,#7179,.F.) ;
#9364 = ORIENTED_EDGE('',*,*,#7180,.T.) ;
#9365 = ORIENTED_EDGE('',*,*,#7181,.F.) ;
#9366 = ORIENTED_EDGE('',*,*,#7182,.T.) ;
#9367 = ORIENTED_EDGE('',*,*,#7183,.F.) ;
#9368 = ORIENTED_EDGE('',*,*,#7184,.T.) ;
#9369 = ORIENTED_EDGE('',*,*,#7185,.F.) ;
#9370 = ORIENTED_EDGE('',*,*,#7186,.T.) ;
#9371 = ORIENTED_EDGE('',*,*,#7187,.F.) ;
#9372 = ORIENTED_EDGE('',*,*,#7188,.T.) ;
#9373 = ORIENTED_EDGE('',*,*,#7189,.F.) ;
#9374 = ORIENTED_EDGE('',*,*,#7190,.T.) ;
#9375 = ORIENTED_EDGE('',*,*,#7191,.F.) ;
#9376 = ORIENTED_EDGE('',*,*,#7192,.T.) ;
#9377 = ORIENTED_EDGE('',*,*,#7193,.F.) ;
#9378 = ORIENTED_EDGE('',*,*,#7194,.T.) ;
#9379 = ORIENTED_EDGE('',*,*,#7195,.F.) ;
#9380 = ORIENTED_EDGE('',*,*,#7196,.T.) ;
#9381 = ORIENTED_EDGE('',*,*,#7197,.F.) ;
#9382 = ORIENTED_EDGE('',*,*,#7198,.T.) ;
#9383 = ORIENTED_EDGE('',*,*,#7199,.F.) ;
#9384 = ORIENTED_EDGE('',*,*,#7200,.T.) ;
#9385 = ORIENTED_EDGE('',*,*,#7201,.F.) ;
#9386 = ORIENTED_EDGE('',*,*,#7202,.T.) ;
#9387 = ORIENTED_EDGE('',*,*,#7203,.F.) ;
#9388 = ORIENTED_EDGE('',*,*,#7204,.T.) ;
#9389 = ORIENTED_EDGE('',*,*,#7205,.F.) ;
#9390 = ORIENTED_EDGE('',*,*,#7206,.T.) ;
#9391 = ORIENTED_EDGE('',*,*,#7207,.F.) ;
#9392 = ORIENTED_EDGE('',*,*,#7208,.T.) ;
#9393 = ORIENTED_EDGE('',*,*,#7209,.F.) ;
#9394 = ORIENTED_EDGE('',*,*,#7210,.T.) ;
#9395 = ORIENTED_EDGE('',*,*,#7211,.F.) ;
#9396 = ORIENTED_EDGE('',*,*,#7212,.T.) ;
#9397 = ORIENTED_EDGE('',*,*,#7213,.F.) ;
#9398 = ORIENTED_EDGE('',*,*,#7214,.T.) ;
#9399 = ORIENTED_EDGE('',*,*,#7215,.F.) ;
#9400 = ORIENTED_EDGE('',*,*,#7216,.T.) ;
#9401 = ORIENTED_EDGE('',*,*,#7217,.F.) ;
#9402 = ORIENTED_EDGE('',*,*,#7218,.T.) ;
#9403 = ORIENTED_EDGE('',*,*,#7219,.F.) ;
#9404 = ORIENTED_EDGE('',*,*,#7220,.T.) ;
#9405 = ORIENTED_EDGE('',*,*,#7221,.F.) ;
#9406 = ORIENTED_EDGE('',*,*,#7176,.T.) ;
#9407 = ORIENTED_EDGE('',*,*,#7170,.F.) ;
#9408 = ORIENTED_EDGE('',*,*,#7172,.T.) ;
#9409 = ORIENTED_EDGE('',*,*,#7164,.F.) ;
#9410 = ORIENTED_EDGE('',*,*,#7150,.T.) ;
#9411 = ORIENTED_EDGE('',*,*,#7162,.T.) ;
#9412 = ORIENTED_EDGE('',*,*,#7154,.T.) ;
#9413 = ORIENTED_EDGE('',*,*,#7158,.T.) ;
#9414 = ORIENTED_EDGE('',*,*,#7174,.F.) ;
#9415 = ORIENTED_EDGE('',*,*,#7222,.T.) ;
#9416 = ORIENTED_EDGE('',*,*,#7223,.T.) ;
#9417 = ORIENTED_EDGE('',*,*,#7179,.T.) ;
#9418 = ORIENTED_EDGE('',*,*,#7224,.F.) ;
#9419 = ORIENTED_EDGE('',*,*,#7181,.T.) ;
#9420 = ORIENTED_EDGE('',*,*,#7225,.T.) ;
#9421 = ORIENTED_EDGE('',*,*,#7226,.T.) ;
#9422 = ORIENTED_EDGE('',*,*,#7227,.T.) ;
#9423 = ORIENTED_EDGE('',*,*,#7225,.F.) ;
#9424 = ORIENTED_EDGE('',*,*,#7180,.F.) ;
#9425 = ORIENTED_EDGE('',*,*,#7223,.F.) ;
#9426 = ORIENTED_EDGE('',*,*,#7224,.T.) ;
#9427 = ORIENTED_EDGE('',*,*,#7228,.F.) ;
#9428 = ORIENTED_EDGE('',*,*,#7229,.T.) ;
#9429 = ORIENTED_EDGE('',*,*,#7182,.F.) ;
#9430 = ORIENTED_EDGE('',*,*,#7230,.F.) ;
#9431 = ORIENTED_EDGE('',*,*,#7185,.T.) ;
#9432 = ORIENTED_EDGE('',*,*,#7231,.T.) ;
#9433 = ORIENTED_EDGE('',*,*,#7232,.T.) ;
#9434 = ORIENTED_EDGE('',*,*,#7229,.F.) ;
#9435 = ORIENTED_EDGE('',*,*,#7233,.T.) ;
#9436 = ORIENTED_EDGE('',*,*,#7234,.T.) ;
#9437 = ORIENTED_EDGE('',*,*,#7183,.T.) ;
#9438 = ORIENTED_EDGE('',*,*,#7235,.T.) ;
#9439 = ORIENTED_EDGE('',*,*,#7231,.F.) ;
#9440 = ORIENTED_EDGE('',*,*,#7184,.F.) ;
#9441 = ORIENTED_EDGE('',*,*,#7234,.F.) ;
#9442 = ORIENTED_EDGE('',*,*,#7230,.T.) ;
#9443 = ORIENTED_EDGE('',*,*,#7236,.F.) ;
#9444 = ORIENTED_EDGE('',*,*,#7237,.T.) ;
#9445 = ORIENTED_EDGE('',*,*,#7186,.F.) ;
#9446 = ORIENTED_EDGE('',*,*,#7237,.F.) ;
#9447 = ORIENTED_EDGE('',*,*,#7238,.T.) ;
#9448 = ORIENTED_EDGE('',*,*,#7239,.T.) ;
#9449 = ORIENTED_EDGE('',*,*,#7187,.T.) ;
#9450 = ORIENTED_EDGE('',*,*,#7240,.F.) ;
#9451 = ORIENTED_EDGE('',*,*,#7189,.T.) ;
#9452 = ORIENTED_EDGE('',*,*,#7241,.T.) ;
#9453 = ORIENTED_EDGE('',*,*,#7242,.T.) ;
#9454 = ORIENTED_EDGE('',*,*,#7243,.T.) ;
#9455 = ORIENTED_EDGE('',*,*,#7241,.F.) ;
#9456 = ORIENTED_EDGE('',*,*,#7188,.F.) ;
#9457 = ORIENTED_EDGE('',*,*,#7239,.F.) ;
#9458 = ORIENTED_EDGE('',*,*,#7240,.T.) ;
#9459 = ORIENTED_EDGE('',*,*,#7244,.F.) ;
#9460 = ORIENTED_EDGE('',*,*,#7245,.T.) ;
#9461 = ORIENTED_EDGE('',*,*,#7190,.F.) ;
#9462 = ORIENTED_EDGE('',*,*,#7246,.F.) ;
#9463 = ORIENTED_EDGE('',*,*,#7193,.T.) ;
#9464 = ORIENTED_EDGE('',*,*,#7247,.T.) ;
#9465 = ORIENTED_EDGE('',*,*,#7248,.T.) ;
#9466 = ORIENTED_EDGE('',*,*,#7245,.F.) ;
#9467 = ORIENTED_EDGE('',*,*,#7249,.T.) ;
#9468 = ORIENTED_EDGE('',*,*,#7250,.T.) ;
#9469 = ORIENTED_EDGE('',*,*,#7191,.T.) ;
#9470 = ORIENTED_EDGE('',*,*,#7251,.T.) ;
#9471 = ORIENTED_EDGE('',*,*,#7247,.F.) ;
#9472 = ORIENTED_EDGE('',*,*,#7192,.F.) ;
#9473 = ORIENTED_EDGE('',*,*,#7250,.F.) ;
#9474 = ORIENTED_EDGE('',*,*,#7246,.T.) ;
#9475 = ORIENTED_EDGE('',*,*,#7252,.F.) ;
#9476 = ORIENTED_EDGE('',*,*,#7253,.T.) ;
#9477 = ORIENTED_EDGE('',*,*,#7194,.F.) ;
#9478 = ORIENTED_EDGE('',*,*,#7253,.F.) ;
#9479 = ORIENTED_EDGE('',*,*,#7254,.T.) ;
#9480 = ORIENTED_EDGE('',*,*,#7255,.T.) ;
#9481 = ORIENTED_EDGE('',*,*,#7195,.T.) ;
#9482 = ORIENTED_EDGE('',*,*,#7256,.F.) ;
#9483 = ORIENTED_EDGE('',*,*,#7197,.T.) ;
#9484 = ORIENTED_EDGE('',*,*,#7257,.T.) ;
#9485 = ORIENTED_EDGE('',*,*,#7258,.T.) ;
#9486 = ORIENTED_EDGE('',*,*,#7259,.T.) ;
#9487 = ORIENTED_EDGE('',*,*,#7257,.F.) ;
#9488 = ORIENTED_EDGE('',*,*,#7196,.F.) ;
#9489 = ORIENTED_EDGE('',*,*,#7255,.F.) ;
#9490 = ORIENTED_EDGE('',*,*,#7256,.T.) ;
#9491 = ORIENTED_EDGE('',*,*,#7260,.F.) ;
#9492 = ORIENTED_EDGE('',*,*,#7261,.T.) ;
#9493 = ORIENTED_EDGE('',*,*,#7198,.F.) ;
#9494 = ORIENTED_EDGE('',*,*,#7262,.F.) ;
#9495 = ORIENTED_EDGE('',*,*,#7201,.T.) ;
#9496 = ORIENTED_EDGE('',*,*,#7263,.T.) ;
#9497 = ORIENTED_EDGE('',*,*,#7264,.T.) ;
#9498 = ORIENTED_EDGE('',*,*,#7261,.F.) ;
#9499 = ORIENTED_EDGE('',*,*,#7265,.T.) ;
#9500 = ORIENTED_EDGE('',*,*,#7266,.T.) ;
#9501 = ORIENTED_EDGE('',*,*,#7199,.T.) ;
#9502 = ORIENTED_EDGE('',*,*,#7267,.T.) ;
#9503 = ORIENTED_EDGE('',*,*,#7263,.F.) ;
#9504 = ORIENTED_EDGE('',*,*,#7200,.F.) ;
#9505 = ORIENTED_EDGE('',*,*,#7266,.F.) ;
#9506 = ORIENTED_EDGE('',*,*,#7262,.T.) ;
#9507 = ORIENTED_EDGE('',*,*,#7268,.F.) ;
#9508 = ORIENTED_EDGE('',*,*,#7269,.T.) ;
#9509 = ORIENTED_EDGE('',*,*,#7202,.F.) ;
#9510 = ORIENTED_EDGE('',*,*,#7269,.F.) ;
#9511 = ORIENTED_EDGE('',*,*,#7270,.T.) ;
#9512 = ORIENTED_EDGE('',*,*,#7271,.T.) ;
#9513 = ORIENTED_EDGE('',*,*,#7203,.T.) ;
#9514 = ORIENTED_EDGE('',*,*,#7272,.F.) ;
#9515 = ORIENTED_EDGE('',*,*,#7205,.T.) ;
#9516 = ORIENTED_EDGE('',*,*,#7273,.T.) ;
#9517 = ORIENTED_EDGE('',*,*,#7274,.T.) ;
#9518 = ORIENTED_EDGE('',*,*,#7275,.T.) ;
#9519 = ORIENTED_EDGE('',*,*,#7273,.F.) ;
#9520 = ORIENTED_EDGE('',*,*,#7204,.F.) ;
#9521 = ORIENTED_EDGE('',*,*,#7271,.F.) ;
#9522 = ORIENTED_EDGE('',*,*,#7272,.T.) ;
#9523 = ORIENTED_EDGE('',*,*,#7276,.F.) ;
#9524 = ORIENTED_EDGE('',*,*,#7277,.T.) ;
#9525 = ORIENTED_EDGE('',*,*,#7206,.F.) ;
#9526 = ORIENTED_EDGE('',*,*,#7278,.F.) ;
#9527 = ORIENTED_EDGE('',*,*,#7209,.T.) ;
#9528 = ORIENTED_EDGE('',*,*,#7279,.T.) ;
#9529 = ORIENTED_EDGE('',*,*,#7280,.T.) ;
#9530 = ORIENTED_EDGE('',*,*,#7277,.F.) ;
#9531 = ORIENTED_EDGE('',*,*,#7281,.T.) ;
#9532 = ORIENTED_EDGE('',*,*,#7282,.T.) ;
#9533 = ORIENTED_EDGE('',*,*,#7207,.T.) ;
#9534 = ORIENTED_EDGE('',*,*,#7283,.T.) ;
#9535 = ORIENTED_EDGE('',*,*,#7279,.F.) ;
#9536 = ORIENTED_EDGE('',*,*,#7208,.F.) ;
#9537 = ORIENTED_EDGE('',*,*,#7282,.F.) ;
#9538 = ORIENTED_EDGE('',*,*,#7278,.T.) ;
#9539 = ORIENTED_EDGE('',*,*,#7284,.F.) ;
#9540 = ORIENTED_EDGE('',*,*,#7285,.T.) ;
#9541 = ORIENTED_EDGE('',*,*,#7210,.F.) ;
#9542 = ORIENTED_EDGE('',*,*,#7285,.F.) ;
#9543 = ORIENTED_EDGE('',*,*,#7286,.T.) ;
#9544 = ORIENTED_EDGE('',*,*,#7287,.T.) ;
#9545 = ORIENTED_EDGE('',*,*,#7211,.T.) ;
#9546 = ORIENTED_EDGE('',*,*,#7288,.F.) ;
#9547 = ORIENTED_EDGE('',*,*,#7213,.T.) ;
#9548 = ORIENTED_EDGE('',*,*,#7289,.T.) ;
#9549 = ORIENTED_EDGE('',*,*,#7290,.T.) ;
#9550 = ORIENTED_EDGE('',*,*,#7291,.T.) ;
#9551 = ORIENTED_EDGE('',*,*,#7289,.F.) ;
#9552 = ORIENTED_EDGE('',*,*,#7212,.F.) ;
#9553 = ORIENTED_EDGE('',*,*,#7287,.F.) ;
#9554 = ORIENTED_EDGE('',*,*,#7288,.T.) ;
#9555 = ORIENTED_EDGE('',*,*,#7292,.F.) ;
#9556 = ORIENTED_EDGE('',*,*,#7293,.T.) ;
#9557 = ORIENTED_EDGE('',*,*,#7214,.F.) ;
#9558 = ORIENTED_EDGE('',*,*,#7294,.F.) ;
#9559 = ORIENTED_EDGE('',*,*,#7217,.T.) ;
#9560 = ORIENTED_EDGE('',*,*,#7295,.T.) ;
#9561 = ORIENTED_EDGE('',*,*,#7296,.T.) ;
#9562 = ORIENTED_EDGE('',*,*,#7293,.F.) ;
#9563 = ORIENTED_EDGE('',*,*,#7297,.T.) ;
#9564 = ORIENTED_EDGE('',*,*,#7298,.T.) ;
#9565 = ORIENTED_EDGE('',*,*,#7215,.T.) ;
#9566 = ORIENTED_EDGE('',*,*,#7299,.T.) ;
#9567 = ORIENTED_EDGE('',*,*,#7295,.F.) ;
#9568 = ORIENTED_EDGE('',*,*,#7216,.F.) ;
#9569 = ORIENTED_EDGE('',*,*,#7298,.F.) ;
#9570 = ORIENTED_EDGE('',*,*,#7294,.T.) ;
#9571 = ORIENTED_EDGE('',*,*,#7300,.F.) ;
#9572 = ORIENTED_EDGE('',*,*,#7301,.T.) ;
#9573 = ORIENTED_EDGE('',*,*,#7218,.F.) ;
#9574 = ORIENTED_EDGE('',*,*,#7301,.F.) ;
#9575 = ORIENTED_EDGE('',*,*,#7302,.T.) ;
#9576 = ORIENTED_EDGE('',*,*,#7303,.T.) ;
#9577 = ORIENTED_EDGE('',*,*,#7219,.T.) ;
#9578 = ORIENTED_EDGE('',*,*,#7177,.F.) ;
#9579 = ORIENTED_EDGE('',*,*,#7221,.T.) ;
#9580 = ORIENTED_EDGE('',*,*,#7304,.T.) ;
#9581 = ORIENTED_EDGE('',*,*,#7305,.T.) ;
#9582 = ORIENTED_EDGE('',*,*,#7306,.T.) ;
#9583 = ORIENTED_EDGE('',*,*,#7304,.F.) ;
#9584 = ORIENTED_EDGE('',*,*,#7220,.F.) ;
#9585 = ORIENTED_EDGE('',*,*,#7303,.F.) ;
#9586 = ORIENTED_EDGE('',*,*,#7307,.F.) ;
#9587 = ORIENTED_EDGE('',*,*,#7308,.T.) ;
#9588 = ORIENTED_EDGE('',*,*,#7160,.F.) ;
#9589 = ORIENTED_EDGE('',*,*,#7308,.F.) ;
#9590 = ORIENTED_EDGE('',*,*,#7178,.T.) ;
#9591 = ORIENTED_EDGE('',*,*,#7305,.F.) ;
#9592 = ORIENTED_EDGE('',*,*,#7306,.F.) ;
#9593 = ORIENTED_EDGE('',*,*,#7302,.F.) ;
#9594 = ORIENTED_EDGE('',*,*,#7300,.T.) ;
#9595 = ORIENTED_EDGE('',*,*,#7296,.F.) ;
#9596 = ORIENTED_EDGE('',*,*,#7299,.F.) ;
#9597 = ORIENTED_EDGE('',*,*,#7297,.F.) ;
#9598 = ORIENTED_EDGE('',*,*,#7292,.T.) ;
#9599 = ORIENTED_EDGE('',*,*,#7290,.F.) ;
#9600 = ORIENTED_EDGE('',*,*,#7291,.F.) ;
#9601 = ORIENTED_EDGE('',*,*,#7286,.F.) ;
#9602 = ORIENTED_EDGE('',*,*,#7284,.T.) ;
#9603 = ORIENTED_EDGE('',*,*,#7280,.F.) ;
#9604 = ORIENTED_EDGE('',*,*,#7283,.F.) ;
#9605 = ORIENTED_EDGE('',*,*,#7281,.F.) ;
#9606 = ORIENTED_EDGE('',*,*,#7276,.T.) ;
#9607 = ORIENTED_EDGE('',*,*,#7274,.F.) ;
#9608 = ORIENTED_EDGE('',*,*,#7275,.F.) ;
#9609 = ORIENTED_EDGE('',*,*,#7270,.F.) ;
#9610 = ORIENTED_EDGE('',*,*,#7268,.T.) ;
#9611 = ORIENTED_EDGE('',*,*,#7264,.F.) ;
#9612 = ORIENTED_EDGE('',*,*,#7267,.F.) ;
#9613 = ORIENTED_EDGE('',*,*,#7265,.F.) ;
#9614 = ORIENTED_EDGE('',*,*,#7260,.T.) ;
#9615 = ORIENTED_EDGE('',*,*,#7258,.F.) ;
#9616 = ORIENTED_EDGE('',*,*,#7259,.F.) ;
#9617 = ORIENTED_EDGE('',*,*,#7254,.F.) ;
#9618 = ORIENTED_EDGE('',*,*,#7252,.T.) ;
#9619 = ORIENTED_EDGE('',*,*,#7248,.F.) ;
#9620 = ORIENTED_EDGE('',*,*,#7251,.F.) ;
#9621 = ORIENTED_EDGE('',*,*,#7249,.F.) ;
#9622 = ORIENTED_EDGE('',*,*,#7244,.T.) ;
#9623 = ORIENTED_EDGE('',*,*,#7242,.F.) ;
#9624 = ORIENTED_EDGE('',*,*,#7243,.F.) ;
#9625 = ORIENTED_EDGE('',*,*,#7238,.F.) ;
#9626 = ORIENTED_EDGE('',*,*,#7236,.T.) ;
#9627 = ORIENTED_EDGE('',*,*,#7232,.F.) ;
#9628 = ORIENTED_EDGE('',*,*,#7235,.F.) ;
#9629 = ORIENTED_EDGE('',*,*,#7233,.F.) ;
#9630 = ORIENTED_EDGE('',*,*,#7228,.T.) ;
#9631 = ORIENTED_EDGE('',*,*,#7226,.F.) ;
#9632 = ORIENTED_EDGE('',*,*,#7227,.F.) ;
#9633 = ORIENTED_EDGE('',*,*,#7222,.F.) ;
#9634 = ORIENTED_EDGE('',*,*,#7173,.T.) ;
#9635 = ORIENTED_EDGE('',*,*,#7166,.F.) ;
#9636 = ORIENTED_EDGE('',*,*,#7171,.F.) ;
#9637 = ORIENTED_EDGE('',*,*,#7168,.F.) ;
#9638 = ORIENTED_EDGE('',*,*,#7307,.T.) ;
#9639 = ORIENTED_EDGE('',*,*,#7309,.T.) ;
#9640 = ORIENTED_EDGE('',*,*,#7310,.T.) ;
#9641 = ORIENTED_EDGE('',*,*,#7311,.T.) ;
#9642 = ORIENTED_EDGE('',*,*,#7312,.T.) ;
#9643 = ORIENTED_EDGE('',*,*,#7313,.T.) ;
#9644 = ORIENTED_EDGE('',*,*,#7314,.T.) ;
#9645 = ORIENTED_EDGE('',*,*,#7315,.T.) ;
#9646 = ORIENTED_EDGE('',*,*,#7316,.T.) ;
#9647 = ORIENTED_EDGE('',*,*,#7317,.T.) ;
#9648 = ORIENTED_EDGE('',*,*,#7314,.F.) ;
#9649 = ORIENTED_EDGE('',*,*,#7318,.F.) ;
#9650 = ORIENTED_EDGE('',*,*,#7312,.F.) ;
#9651 = ORIENTED_EDGE('',*,*,#7319,.T.) ;
#9652 = ORIENTED_EDGE('',*,*,#7315,.F.) ;
#9653 = ORIENTED_EDGE('',*,*,#7317,.F.) ;
#9654 = ORIENTED_EDGE('',*,*,#7311,.F.) ;
#9655 = ORIENTED_EDGE('',*,*,#7320,.T.) ;
#9656 = ORIENTED_EDGE('',*,*,#7316,.F.) ;
#9657 = ORIENTED_EDGE('',*,*,#7319,.F.) ;
#9658 = ORIENTED_EDGE('',*,*,#7310,.F.) ;
#9659 = ORIENTED_EDGE('',*,*,#7318,.T.) ;
#9660 = ORIENTED_EDGE('',*,*,#7313,.F.) ;
#9661 = ORIENTED_EDGE('',*,*,#7320,.F.) ;
#9662 = ORIENTED_EDGE('',*,*,#7309,.F.) ;
#9663 = ORIENTED_EDGE('',*,*,#7321,.F.) ;
#9664 = ORIENTED_EDGE('',*,*,#7322,.T.) ;
#9665 = ORIENTED_EDGE('',*,*,#7323,.F.) ;
#9666 = ORIENTED_EDGE('',*,*,#7322,.F.) ;
#9667 = ORIENTED_EDGE('',*,*,#7324,.F.) ;
#9668 = ORIENTED_EDGE('',*,*,#7325,.T.) ;
#9669 = ORIENTED_EDGE('',*,*,#7326,.F.) ;
#9670 = ORIENTED_EDGE('',*,*,#7325,.F.) ;
#9671 = ORIENTED_EDGE('',*,*,#7326,.T.) ;
#9672 = ORIENTED_EDGE('',*,*,#7321,.T.) ;
#9673 = ORIENTED_EDGE('',*,*,#7324,.T.) ;
#9674 = ORIENTED_EDGE('',*,*,#7323,.T.) ;
#9675 = ORIENTED_EDGE('',*,*,#7327,.F.) ;
#9676 = ORIENTED_EDGE('',*,*,#7328,.F.) ;
#9677 = ORIENTED_EDGE('',*,*,#7329,.F.) ;
#9678 = ORIENTED_EDGE('',*,*,#7330,.F.) ;
#9679 = ORIENTED_EDGE('',*,*,#7331,.F.) ;
#9680 = ORIENTED_EDGE('',*,*,#7330,.T.) ;
#9681 = ORIENTED_EDGE('',*,*,#7332,.F.) ;
#9682 = ORIENTED_EDGE('',*,*,#7333,.F.) ;
#9683 = ORIENTED_EDGE('',*,*,#7334,.F.) ;
#9684 = ORIENTED_EDGE('',*,*,#7332,.T.) ;
#9685 = ORIENTED_EDGE('',*,*,#7329,.T.) ;
#9686 = ORIENTED_EDGE('',*,*,#7335,.F.) ;
#9687 = ORIENTED_EDGE('',*,*,#7336,.F.) ;
#9688 = ORIENTED_EDGE('',*,*,#7337,.F.) ;
#9689 = ORIENTED_EDGE('',*,*,#7335,.T.) ;
#9690 = ORIENTED_EDGE('',*,*,#7328,.T.) ;
#9691 = ORIENTED_EDGE('',*,*,#7336,.T.) ;
#9692 = ORIENTED_EDGE('',*,*,#7327,.T.) ;
#9693 = ORIENTED_EDGE('',*,*,#7331,.T.) ;
#9694 = ORIENTED_EDGE('',*,*,#7338,.F.) ;
#9695 = ORIENTED_EDGE('',*,*,#7339,.T.) ;
#9696 = ORIENTED_EDGE('',*,*,#7340,.F.) ;
#9697 = ORIENTED_EDGE('',*,*,#7341,.F.) ;
#9698 = ORIENTED_EDGE('',*,*,#7342,.F.) ;
#9699 = ORIENTED_EDGE('',*,*,#7337,.T.) ;
#9700 = ORIENTED_EDGE('',*,*,#7342,.T.) ;
#9701 = ORIENTED_EDGE('',*,*,#7343,.T.) ;
#9702 = ORIENTED_EDGE('',*,*,#7344,.T.) ;
#9703 = ORIENTED_EDGE('',*,*,#7345,.T.) ;
#9704 = ORIENTED_EDGE('',*,*,#7338,.T.) ;
#9705 = ORIENTED_EDGE('',*,*,#7333,.T.) ;
#9706 = ORIENTED_EDGE('',*,*,#7334,.T.) ;
#9707 = ORIENTED_EDGE('',*,*,#7346,.T.) ;
#9708 = ORIENTED_EDGE('',*,*,#7347,.T.) ;
#9709 = ORIENTED_EDGE('',*,*,#7348,.T.) ;
#9710 = ORIENTED_EDGE('',*,*,#7340,.T.) ;
#9711 = ORIENTED_EDGE('',*,*,#7349,.T.) ;
#9712 = ORIENTED_EDGE('',*,*,#7347,.F.) ;
#9713 = ORIENTED_EDGE('',*,*,#7350,.F.) ;
#9714 = ORIENTED_EDGE('',*,*,#7344,.F.) ;
#9715 = ORIENTED_EDGE('',*,*,#7341,.T.) ;
#9716 = ORIENTED_EDGE('',*,*,#7348,.F.) ;
#9717 = ORIENTED_EDGE('',*,*,#7349,.F.) ;
#9718 = ORIENTED_EDGE('',*,*,#7343,.F.) ;
#9719 = ORIENTED_EDGE('',*,*,#7350,.T.) ;
#9720 = ORIENTED_EDGE('',*,*,#7346,.F.) ;
#9721 = ORIENTED_EDGE('',*,*,#7339,.F.) ;
#9722 = ORIENTED_EDGE('',*,*,#7345,.F.) ;
#9723 = ORIENTED_EDGE('',*,*,#7351,.F.) ;
#9724 = ORIENTED_EDGE('',*,*,#7352,.T.) ;
#9725 = ORIENTED_EDGE('',*,*,#7353,.F.) ;
#9726 = ORIENTED_EDGE('',*,*,#7352,.F.) ;
#9727 = ORIENTED_EDGE('',*,*,#7353,.T.) ;
#9728 = ORIENTED_EDGE('',*,*,#7354,.F.) ;
#9729 = ORIENTED_EDGE('',*,*,#7355,.T.) ;
#9730 = ORIENTED_EDGE('',*,*,#7356,.F.) ;
#9731 = ORIENTED_EDGE('',*,*,#7355,.F.) ;
#9732 = ORIENTED_EDGE('',*,*,#7357,.F.) ;
#9733 = ORIENTED_EDGE('',*,*,#7358,.F.) ;
#9734 = ORIENTED_EDGE('',*,*,#7359,.F.) ;
#9735 = ORIENTED_EDGE('',*,*,#7360,.F.) ;
#9736 = ORIENTED_EDGE('',*,*,#7361,.F.) ;
#9737 = ORIENTED_EDGE('',*,*,#7362,.F.) ;
#9738 = ORIENTED_EDGE('',*,*,#7363,.F.) ;
#9739 = ORIENTED_EDGE('',*,*,#7364,.F.) ;
#9740 = ORIENTED_EDGE('',*,*,#7365,.F.) ;
#9741 = ORIENTED_EDGE('',*,*,#7366,.F.) ;
#9742 = ORIENTED_EDGE('',*,*,#7367,.F.) ;
#9743 = ORIENTED_EDGE('',*,*,#7368,.F.) ;
#9744 = ORIENTED_EDGE('',*,*,#7367,.T.) ;
#9745 = ORIENTED_EDGE('',*,*,#7369,.T.) ;
#9746 = ORIENTED_EDGE('',*,*,#7370,.T.) ;
#9747 = ORIENTED_EDGE('',*,*,#7371,.T.) ;
#9748 = ORIENTED_EDGE('',*,*,#7365,.T.) ;
#9749 = ORIENTED_EDGE('',*,*,#7372,.T.) ;
#9750 = ORIENTED_EDGE('',*,*,#7373,.T.) ;
#9751 = ORIENTED_EDGE('',*,*,#7374,.T.) ;
#9752 = ORIENTED_EDGE('',*,*,#7363,.T.) ;
#9753 = ORIENTED_EDGE('',*,*,#7375,.T.) ;
#9754 = ORIENTED_EDGE('',*,*,#7376,.F.) ;
#9755 = ORIENTED_EDGE('',*,*,#7377,.F.) ;
#9756 = ORIENTED_EDGE('',*,*,#7378,.F.) ;
#9757 = ORIENTED_EDGE('',*,*,#7372,.F.) ;
#9758 = ORIENTED_EDGE('',*,*,#7368,.T.) ;
#9759 = ORIENTED_EDGE('',*,*,#7371,.F.) ;
#9760 = ORIENTED_EDGE('',*,*,#7379,.T.) ;
#9761 = ORIENTED_EDGE('',*,*,#7380,.F.) ;
#9762 = ORIENTED_EDGE('',*,*,#7360,.T.) ;
#9763 = ORIENTED_EDGE('',*,*,#7381,.F.) ;
#9764 = ORIENTED_EDGE('',*,*,#7375,.F.) ;
#9765 = ORIENTED_EDGE('',*,*,#7362,.T.) ;
#9766 = ORIENTED_EDGE('',*,*,#7356,.T.) ;
#9767 = ORIENTED_EDGE('',*,*,#7359,.T.) ;
#9768 = ORIENTED_EDGE('',*,*,#7382,.T.) ;
#9769 = ORIENTED_EDGE('',*,*,#7376,.T.) ;
#9770 = ORIENTED_EDGE('',*,*,#7381,.T.) ;
#9771 = ORIENTED_EDGE('',*,*,#7357,.T.) ;
#9772 = ORIENTED_EDGE('',*,*,#7380,.T.) ;
#9773 = ORIENTED_EDGE('',*,*,#7383,.T.) ;
#9774 = ORIENTED_EDGE('',*,*,#7384,.T.) ;
#9775 = ORIENTED_EDGE('',*,*,#7374,.F.) ;
#9776 = ORIENTED_EDGE('',*,*,#7385,.T.) ;
#9777 = ORIENTED_EDGE('',*,*,#7364,.T.) ;
#9778 = ORIENTED_EDGE('',*,*,#7377,.T.) ;
#9779 = ORIENTED_EDGE('',*,*,#7382,.F.) ;
#9780 = ORIENTED_EDGE('',*,*,#7358,.T.) ;
#9781 = ORIENTED_EDGE('',*,*,#7384,.F.) ;
#9782 = ORIENTED_EDGE('',*,*,#7386,.F.) ;
#9783 = ORIENTED_EDGE('',*,*,#7369,.F.) ;
#9784 = ORIENTED_EDGE('',*,*,#7366,.T.) ;
#9785 = ORIENTED_EDGE('',*,*,#7351,.T.) ;
#9786 = ORIENTED_EDGE('',*,*,#7354,.T.) ;
#9787 = ORIENTED_EDGE('',*,*,#7361,.T.) ;
#9788 = ORIENTED_EDGE('',*,*,#7385,.F.) ;
#9789 = ORIENTED_EDGE('',*,*,#7373,.F.) ;
#9790 = ORIENTED_EDGE('',*,*,#7378,.T.) ;
#9791 = ORIENTED_EDGE('',*,*,#7386,.T.) ;
#9792 = ORIENTED_EDGE('',*,*,#7383,.F.) ;
#9793 = ORIENTED_EDGE('',*,*,#7379,.F.) ;
#9794 = ORIENTED_EDGE('',*,*,#7370,.F.) ;
#9795 = ORIENTED_EDGE('',*,*,#7387,.F.) ;
#9796 = ORIENTED_EDGE('',*,*,#7388,.T.) ;
#9797 = ORIENTED_EDGE('',*,*,#7389,.F.) ;
#9798 = ORIENTED_EDGE('',*,*,#7388,.F.) ;
#9799 = ORIENTED_EDGE('',*,*,#7389,.T.) ;
#9800 = ORIENTED_EDGE('',*,*,#7387,.T.) ;
#9801 = ORIENTED_EDGE('',*,*,#7390,.T.) ;
#9802 = ORIENTED_EDGE('',*,*,#7391,.T.) ;
#9803 = ORIENTED_EDGE('',*,*,#7392,.T.) ;
#9804 = ORIENTED_EDGE('',*,*,#7393,.T.) ;
#9805 = ORIENTED_EDGE('',*,*,#7394,.T.) ;
#9806 = ORIENTED_EDGE('',*,*,#7395,.F.) ;
#9807 = ORIENTED_EDGE('',*,*,#7395,.T.) ;
#9808 = ORIENTED_EDGE('',*,*,#7396,.T.) ;
#9809 = ORIENTED_EDGE('',*,*,#7397,.T.) ;
#9810 = ORIENTED_EDGE('',*,*,#7398,.T.) ;
#9811 = ORIENTED_EDGE('',*,*,#7399,.T.) ;
#9812 = ORIENTED_EDGE('',*,*,#7400,.T.) ;
#9813 = ORIENTED_EDGE('',*,*,#7401,.T.) ;
#9814 = ORIENTED_EDGE('',*,*,#7402,.T.) ;
#9815 = ORIENTED_EDGE('',*,*,#7403,.T.) ;
#9816 = ORIENTED_EDGE('',*,*,#7404,.T.) ;
#9817 = ORIENTED_EDGE('',*,*,#7405,.T.) ;
#9818 = ORIENTED_EDGE('',*,*,#7406,.T.) ;
#9819 = ORIENTED_EDGE('',*,*,#7407,.T.) ;
#9820 = ORIENTED_EDGE('',*,*,#7408,.T.) ;
#9821 = ORIENTED_EDGE('',*,*,#7409,.T.) ;
#9822 = ORIENTED_EDGE('',*,*,#7410,.T.) ;
#9823 = ORIENTED_EDGE('',*,*,#7411,.T.) ;
#9824 = ORIENTED_EDGE('',*,*,#7411,.F.) ;
#9825 = ORIENTED_EDGE('',*,*,#7412,.T.) ;
#9826 = ORIENTED_EDGE('',*,*,#7413,.T.) ;
#9827 = ORIENTED_EDGE('',*,*,#7414,.T.) ;
#9828 = ORIENTED_EDGE('',*,*,#7415,.T.) ;
#9829 = ORIENTED_EDGE('',*,*,#7416,.T.) ;
#9830 = ORIENTED_EDGE('',*,*,#7417,.T.) ;
#9831 = ORIENTED_EDGE('',*,*,#7418,.T.) ;
#9832 = ORIENTED_EDGE('',*,*,#7419,.T.) ;
#9833 = ORIENTED_EDGE('',*,*,#7420,.T.) ;
#9834 = ORIENTED_EDGE('',*,*,#7421,.T.) ;
#9835 = ORIENTED_EDGE('',*,*,#7422,.T.) ;
#9836 = ORIENTED_EDGE('',*,*,#7423,.F.) ;
#9837 = ORIENTED_EDGE('',*,*,#7423,.T.) ;
#9838 = ORIENTED_EDGE('',*,*,#7424,.T.) ;
#9839 = ORIENTED_EDGE('',*,*,#7425,.T.) ;
#9840 = ORIENTED_EDGE('',*,*,#7426,.T.) ;
#9841 = ORIENTED_EDGE('',*,*,#7427,.T.) ;
#9842 = ORIENTED_EDGE('',*,*,#7428,.T.) ;
#9843 = ORIENTED_EDGE('',*,*,#7429,.T.) ;
#9844 = ORIENTED_EDGE('',*,*,#7430,.T.) ;
#9845 = ORIENTED_EDGE('',*,*,#7431,.T.) ;
#9846 = ORIENTED_EDGE('',*,*,#7432,.T.) ;
#9847 = ORIENTED_EDGE('',*,*,#7433,.T.) ;
#9848 = ORIENTED_EDGE('',*,*,#7434,.T.) ;
#9849 = ORIENTED_EDGE('',*,*,#7435,.T.) ;
#9850 = ORIENTED_EDGE('',*,*,#7436,.T.) ;
#9851 = ORIENTED_EDGE('',*,*,#7437,.T.) ;
#9852 = ORIENTED_EDGE('',*,*,#7438,.T.) ;
#9853 = ORIENTED_EDGE('',*,*,#7439,.T.) ;
#9854 = ORIENTED_EDGE('',*,*,#7439,.F.) ;
#9855 = ORIENTED_EDGE('',*,*,#7440,.T.) ;
#9856 = ORIENTED_EDGE('',*,*,#7441,.T.) ;
#9857 = ORIENTED_EDGE('',*,*,#7442,.T.) ;
#9858 = ORIENTED_EDGE('',*,*,#7443,.T.) ;
#9859 = ORIENTED_EDGE('',*,*,#7444,.T.) ;
#9860 = ORIENTED_EDGE('',*,*,#7445,.T.) ;
#9861 = ORIENTED_EDGE('',*,*,#7446,.T.) ;
#9862 = ORIENTED_EDGE('',*,*,#7447,.T.) ;
#9863 = ORIENTED_EDGE('',*,*,#7448,.T.) ;
#9864 = ORIENTED_EDGE('',*,*,#7449,.T.) ;
#9865 = ORIENTED_EDGE('',*,*,#7450,.T.) ;
#9866 = ORIENTED_EDGE('',*,*,#7451,.F.) ;
#9867 = ORIENTED_EDGE('',*,*,#7451,.T.) ;
#9868 = ORIENTED_EDGE('',*,*,#7452,.T.) ;
#9869 = ORIENTED_EDGE('',*,*,#7453,.T.) ;
#9870 = ORIENTED_EDGE('',*,*,#7454,.T.) ;
#9871 = ORIENTED_EDGE('',*,*,#7455,.T.) ;
#9872 = ORIENTED_EDGE('',*,*,#7456,.T.) ;
#9873 = ORIENTED_EDGE('',*,*,#7457,.T.) ;
#9874 = ORIENTED_EDGE('',*,*,#7458,.T.) ;
#9875 = ORIENTED_EDGE('',*,*,#7459,.T.) ;
#9876 = ORIENTED_EDGE('',*,*,#7460,.T.) ;
#9877 = ORIENTED_EDGE('',*,*,#7461,.T.) ;
#9878 = ORIENTED_EDGE('',*,*,#7462,.T.) ;
#9879 = ORIENTED_EDGE('',*,*,#7463,.T.) ;
#9880 = ORIENTED_EDGE('',*,*,#7464,.T.) ;
#9881 = ORIENTED_EDGE('',*,*,#7465,.T.) ;
#9882 = ORIENTED_EDGE('',*,*,#7466,.T.) ;
#9883 = ORIENTED_EDGE('',*,*,#7467,.T.) ;
#9884 = ORIENTED_EDGE('',*,*,#7467,.F.) ;
#9885 = ORIENTED_EDGE('',*,*,#7468,.T.) ;
#9886 = ORIENTED_EDGE('',*,*,#7469,.T.) ;
#9887 = ORIENTED_EDGE('',*,*,#7470,.T.) ;
#9888 = ORIENTED_EDGE('',*,*,#7471,.T.) ;
#9889 = ORIENTED_EDGE('',*,*,#7472,.T.) ;
#9890 = ORIENTED_EDGE('',*,*,#7473,.T.) ;
#9891 = ORIENTED_EDGE('',*,*,#7474,.T.) ;
#9892 = ORIENTED_EDGE('',*,*,#7475,.T.) ;
#9893 = ORIENTED_EDGE('',*,*,#7476,.T.) ;
#9894 = ORIENTED_EDGE('',*,*,#7477,.T.) ;
#9895 = ORIENTED_EDGE('',*,*,#7478,.T.) ;
#9896 = ORIENTED_EDGE('',*,*,#7479,.F.) ;
#9897 = ORIENTED_EDGE('',*,*,#7479,.T.) ;
#9898 = ORIENTED_EDGE('',*,*,#7480,.T.) ;
#9899 = ORIENTED_EDGE('',*,*,#7481,.T.) ;
#9900 = ORIENTED_EDGE('',*,*,#7482,.T.) ;
#9901 = ORIENTED_EDGE('',*,*,#7483,.T.) ;
#9902 = ORIENTED_EDGE('',*,*,#7484,.T.) ;
#9903 = ORIENTED_EDGE('',*,*,#7485,.T.) ;
#9904 = ORIENTED_EDGE('',*,*,#7486,.T.) ;
#9905 = ORIENTED_EDGE('',*,*,#7487,.T.) ;
#9906 = ORIENTED_EDGE('',*,*,#7488,.T.) ;
#9907 = ORIENTED_EDGE('',*,*,#7489,.T.) ;
#9908 = ORIENTED_EDGE('',*,*,#7490,.T.) ;
#9909 = ORIENTED_EDGE('',*,*,#7491,.T.) ;
#9910 = ORIENTED_EDGE('',*,*,#7492,.T.) ;
#9911 = ORIENTED_EDGE('',*,*,#7493,.T.) ;
#9912 = ORIENTED_EDGE('',*,*,#7494,.T.) ;
#9913 = ORIENTED_EDGE('',*,*,#7495,.T.) ;
#9914 = ORIENTED_EDGE('',*,*,#7495,.F.) ;
#9915 = ORIENTED_EDGE('',*,*,#7496,.T.) ;
#9916 = ORIENTED_EDGE('',*,*,#7497,.T.) ;
#9917 = ORIENTED_EDGE('',*,*,#7498,.T.) ;
#9918 = ORIENTED_EDGE('',*,*,#7499,.T.) ;
#9919 = ORIENTED_EDGE('',*,*,#7500,.F.) ;
#9920 = ORIENTED_EDGE('',*,*,#7501,.T.) ;
#9921 = ORIENTED_EDGE('',*,*,#7502,.F.) ;
#9922 = ORIENTED_EDGE('',*,*,#7503,.F.) ;
#9923 = ORIENTED_EDGE('',*,*,#7390,.F.) ;
#9924 = ORIENTED_EDGE('',*,*,#7504,.F.) ;
#9925 = ORIENTED_EDGE('',*,*,#7501,.F.) ;
#9926 = ORIENTED_EDGE('',*,*,#7500,.T.) ;
#9927 = ORIENTED_EDGE('',*,*,#7503,.T.) ;
#9928 = ORIENTED_EDGE('',*,*,#7505,.T.) ;
#9929 = ORIENTED_EDGE('',*,*,#7506,.F.) ;
#9930 = ORIENTED_EDGE('',*,*,#7392,.F.) ;
#9931 = ORIENTED_EDGE('',*,*,#7507,.F.) ;
#9932 = ORIENTED_EDGE('',*,*,#7505,.F.) ;
#9933 = ORIENTED_EDGE('',*,*,#7502,.T.) ;
#9934 = ORIENTED_EDGE('',*,*,#7504,.T.) ;
#9935 = ORIENTED_EDGE('',*,*,#7391,.F.) ;
#9936 = ORIENTED_EDGE('',*,*,#7506,.T.) ;
#9937 = ORIENTED_EDGE('',*,*,#7507,.T.) ;
#9938 = ORIENTED_EDGE('',*,*,#7396,.F.) ;
#9939 = ORIENTED_EDGE('',*,*,#7394,.F.) ;
#9940 = ORIENTED_EDGE('',*,*,#7508,.T.) ;
#9941 = ORIENTED_EDGE('',*,*,#7397,.F.) ;
#9942 = ORIENTED_EDGE('',*,*,#7509,.F.) ;
#9943 = ORIENTED_EDGE('',*,*,#7398,.F.) ;
#9944 = ORIENTED_EDGE('',*,*,#7508,.F.) ;
#9945 = ORIENTED_EDGE('',*,*,#7393,.F.) ;
#9946 = ORIENTED_EDGE('',*,*,#7509,.T.) ;
#9947 = ORIENTED_EDGE('',*,*,#7400,.F.) ;
#9948 = ORIENTED_EDGE('',*,*,#7510,.T.) ;
#9949 = ORIENTED_EDGE('',*,*,#7401,.F.) ;
#9950 = ORIENTED_EDGE('',*,*,#7511,.F.) ;
#9951 = ORIENTED_EDGE('',*,*,#7402,.F.) ;
#9952 = ORIENTED_EDGE('',*,*,#7510,.F.) ;
#9953 = ORIENTED_EDGE('',*,*,#7399,.F.) ;
#9954 = ORIENTED_EDGE('',*,*,#7511,.T.) ;
#9955 = ORIENTED_EDGE('',*,*,#7404,.F.) ;
#9956 = ORIENTED_EDGE('',*,*,#7512,.T.) ;
#9957 = ORIENTED_EDGE('',*,*,#7405,.F.) ;
#9958 = ORIENTED_EDGE('',*,*,#7513,.F.) ;
#9959 = ORIENTED_EDGE('',*,*,#7406,.F.) ;
#9960 = ORIENTED_EDGE('',*,*,#7512,.F.) ;
#9961 = ORIENTED_EDGE('',*,*,#7403,.F.) ;
#9962 = ORIENTED_EDGE('',*,*,#7513,.T.) ;
#9963 = ORIENTED_EDGE('',*,*,#7408,.F.) ;
#9964 = ORIENTED_EDGE('',*,*,#7514,.T.) ;
#9965 = ORIENTED_EDGE('',*,*,#7409,.F.) ;
#9966 = ORIENTED_EDGE('',*,*,#7515,.F.) ;
#9967 = ORIENTED_EDGE('',*,*,#7516,.F.) ;
#9968 = ORIENTED_EDGE('',*,*,#7412,.F.) ;
#9969 = ORIENTED_EDGE('',*,*,#7410,.F.) ;
#9970 = ORIENTED_EDGE('',*,*,#7514,.F.) ;
#9971 = ORIENTED_EDGE('',*,*,#7407,.F.) ;
#9972 = ORIENTED_EDGE('',*,*,#7516,.T.) ;
#9973 = ORIENTED_EDGE('',*,*,#7517,.T.) ;
#9974 = ORIENTED_EDGE('',*,*,#7518,.F.) ;
#9975 = ORIENTED_EDGE('',*,*,#7519,.F.) ;
#9976 = ORIENTED_EDGE('',*,*,#7414,.F.) ;
#9977 = ORIENTED_EDGE('',*,*,#7520,.F.) ;
#9978 = ORIENTED_EDGE('',*,*,#7517,.F.) ;
#9979 = ORIENTED_EDGE('',*,*,#7515,.T.) ;
#9980 = ORIENTED_EDGE('',*,*,#7413,.F.) ;
#9981 = ORIENTED_EDGE('',*,*,#7519,.T.) ;
#9982 = ORIENTED_EDGE('',*,*,#7521,.T.) ;
#9983 = ORIENTED_EDGE('',*,*,#7522,.F.) ;
#9984 = ORIENTED_EDGE('',*,*,#7416,.F.) ;
#9985 = ORIENTED_EDGE('',*,*,#7523,.F.) ;
#9986 = ORIENTED_EDGE('',*,*,#7521,.F.) ;
#9987 = ORIENTED_EDGE('',*,*,#7518,.T.) ;
#9988 = ORIENTED_EDGE('',*,*,#7520,.T.) ;
#9989 = ORIENTED_EDGE('',*,*,#7415,.F.) ;
#9990 = ORIENTED_EDGE('',*,*,#7522,.T.) ;
#9991 = ORIENTED_EDGE('',*,*,#7524,.T.) ;
#9992 = ORIENTED_EDGE('',*,*,#7525,.F.) ;
#9993 = ORIENTED_EDGE('',*,*,#7526,.F.) ;
#9994 = ORIENTED_EDGE('',*,*,#7418,.F.) ;
#9995 = ORIENTED_EDGE('',*,*,#7527,.F.) ;
#9996 = ORIENTED_EDGE('',*,*,#7524,.F.) ;
#9997 = ORIENTED_EDGE('',*,*,#7523,.T.) ;
#9998 = ORIENTED_EDGE('',*,*,#7417,.F.) ;
#9999 = ORIENTED_EDGE('',*,*,#7526,.T.) ;
#10000 = ORIENTED_EDGE('',*,*,#7528,.T.) ;
#10001 = ORIENTED_EDGE('',*,*,#7529,.F.) ;
#10002 = ORIENTED_EDGE('',*,*,#7420,.F.) ;
#10003 = ORIENTED_EDGE('',*,*,#7530,.F.) ;
#10004 = ORIENTED_EDGE('',*,*,#7528,.F.) ;
#10005 = ORIENTED_EDGE('',*,*,#7525,.T.) ;
#10006 = ORIENTED_EDGE('',*,*,#7527,.T.) ;
#10007 = ORIENTED_EDGE('',*,*,#7419,.F.) ;
#10008 = ORIENTED_EDGE('',*,*,#7529,.T.) ;
#10009 = ORIENTED_EDGE('',*,*,#7530,.T.) ;
#10010 = ORIENTED_EDGE('',*,*,#7424,.F.) ;
#10011 = ORIENTED_EDGE('',*,*,#7422,.F.) ;
#10012 = ORIENTED_EDGE('',*,*,#7531,.T.) ;
#10013 = ORIENTED_EDGE('',*,*,#7425,.F.) ;
#10014 = ORIENTED_EDGE('',*,*,#7532,.F.) ;
#10015 = ORIENTED_EDGE('',*,*,#7426,.F.) ;
#10016 = ORIENTED_EDGE('',*,*,#7531,.F.) ;
#10017 = ORIENTED_EDGE('',*,*,#7421,.F.) ;
#10018 = ORIENTED_EDGE('',*,*,#7532,.T.) ;
#10019 = ORIENTED_EDGE('',*,*,#7428,.F.) ;
#10020 = ORIENTED_EDGE('',*,*,#7533,.T.) ;
#10021 = ORIENTED_EDGE('',*,*,#7429,.F.) ;
#10022 = ORIENTED_EDGE('',*,*,#7534,.F.) ;
#10023 = ORIENTED_EDGE('',*,*,#7430,.F.) ;
#10024 = ORIENTED_EDGE('',*,*,#7533,.F.) ;
#10025 = ORIENTED_EDGE('',*,*,#7427,.F.) ;
#10026 = ORIENTED_EDGE('',*,*,#7534,.T.) ;
#10027 = ORIENTED_EDGE('',*,*,#7432,.F.) ;
#10028 = ORIENTED_EDGE('',*,*,#7535,.T.) ;
#10029 = ORIENTED_EDGE('',*,*,#7433,.F.) ;
#10030 = ORIENTED_EDGE('',*,*,#7536,.F.) ;
#10031 = ORIENTED_EDGE('',*,*,#7434,.F.) ;
#10032 = ORIENTED_EDGE('',*,*,#7535,.F.) ;
#10033 = ORIENTED_EDGE('',*,*,#7431,.F.) ;
#10034 = ORIENTED_EDGE('',*,*,#7536,.T.) ;
#10035 = ORIENTED_EDGE('',*,*,#7436,.F.) ;
#10036 = ORIENTED_EDGE('',*,*,#7537,.T.) ;
#10037 = ORIENTED_EDGE('',*,*,#7437,.F.) ;
#10038 = ORIENTED_EDGE('',*,*,#7538,.F.) ;
#10039 = ORIENTED_EDGE('',*,*,#7539,.F.) ;
#10040 = ORIENTED_EDGE('',*,*,#7440,.F.) ;
#10041 = ORIENTED_EDGE('',*,*,#7438,.F.) ;
#10042 = ORIENTED_EDGE('',*,*,#7537,.F.) ;
#10043 = ORIENTED_EDGE('',*,*,#7435,.F.) ;
#10044 = ORIENTED_EDGE('',*,*,#7539,.T.) ;
#10045 = ORIENTED_EDGE('',*,*,#7540,.T.) ;
#10046 = ORIENTED_EDGE('',*,*,#7541,.F.) ;
#10047 = ORIENTED_EDGE('',*,*,#7542,.F.) ;
#10048 = ORIENTED_EDGE('',*,*,#7442,.F.) ;
#10049 = ORIENTED_EDGE('',*,*,#7543,.F.) ;
#10050 = ORIENTED_EDGE('',*,*,#7540,.F.) ;
#10051 = ORIENTED_EDGE('',*,*,#7538,.T.) ;
#10052 = ORIENTED_EDGE('',*,*,#7441,.F.) ;
#10053 = ORIENTED_EDGE('',*,*,#7542,.T.) ;
#10054 = ORIENTED_EDGE('',*,*,#7544,.T.) ;
#10055 = ORIENTED_EDGE('',*,*,#7545,.F.) ;
#10056 = ORIENTED_EDGE('',*,*,#7444,.F.) ;
#10057 = ORIENTED_EDGE('',*,*,#7546,.F.) ;
#10058 = ORIENTED_EDGE('',*,*,#7544,.F.) ;
#10059 = ORIENTED_EDGE('',*,*,#7541,.T.) ;
#10060 = ORIENTED_EDGE('',*,*,#7543,.T.) ;
#10061 = ORIENTED_EDGE('',*,*,#7443,.F.) ;
#10062 = ORIENTED_EDGE('',*,*,#7545,.T.) ;
#10063 = ORIENTED_EDGE('',*,*,#7547,.T.) ;
#10064 = ORIENTED_EDGE('',*,*,#7548,.F.) ;
#10065 = ORIENTED_EDGE('',*,*,#7549,.F.) ;
#10066 = ORIENTED_EDGE('',*,*,#7446,.F.) ;
#10067 = ORIENTED_EDGE('',*,*,#7550,.F.) ;
#10068 = ORIENTED_EDGE('',*,*,#7547,.F.) ;
#10069 = ORIENTED_EDGE('',*,*,#7546,.T.) ;
#10070 = ORIENTED_EDGE('',*,*,#7445,.F.) ;
#10071 = ORIENTED_EDGE('',*,*,#7549,.T.) ;
#10072 = ORIENTED_EDGE('',*,*,#7551,.T.) ;
#10073 = ORIENTED_EDGE('',*,*,#7552,.F.) ;
#10074 = ORIENTED_EDGE('',*,*,#7448,.F.) ;
#10075 = ORIENTED_EDGE('',*,*,#7553,.F.) ;
#10076 = ORIENTED_EDGE('',*,*,#7551,.F.) ;
#10077 = ORIENTED_EDGE('',*,*,#7548,.T.) ;
#10078 = ORIENTED_EDGE('',*,*,#7550,.T.) ;
#10079 = ORIENTED_EDGE('',*,*,#7447,.F.) ;
#10080 = ORIENTED_EDGE('',*,*,#7552,.T.) ;
#10081 = ORIENTED_EDGE('',*,*,#7553,.T.) ;
#10082 = ORIENTED_EDGE('',*,*,#7452,.F.) ;
#10083 = ORIENTED_EDGE('',*,*,#7450,.F.) ;
#10084 = ORIENTED_EDGE('',*,*,#7554,.T.) ;
#10085 = ORIENTED_EDGE('',*,*,#7453,.F.) ;
#10086 = ORIENTED_EDGE('',*,*,#7555,.F.) ;
#10087 = ORIENTED_EDGE('',*,*,#7454,.F.) ;
#10088 = ORIENTED_EDGE('',*,*,#7554,.F.) ;
#10089 = ORIENTED_EDGE('',*,*,#7449,.F.) ;
#10090 = ORIENTED_EDGE('',*,*,#7555,.T.) ;
#10091 = ORIENTED_EDGE('',*,*,#7456,.F.) ;
#10092 = ORIENTED_EDGE('',*,*,#7556,.T.) ;
#10093 = ORIENTED_EDGE('',*,*,#7457,.F.) ;
#10094 = ORIENTED_EDGE('',*,*,#7557,.F.) ;
#10095 = ORIENTED_EDGE('',*,*,#7458,.F.) ;
#10096 = ORIENTED_EDGE('',*,*,#7556,.F.) ;
#10097 = ORIENTED_EDGE('',*,*,#7455,.F.) ;
#10098 = ORIENTED_EDGE('',*,*,#7557,.T.) ;
#10099 = ORIENTED_EDGE('',*,*,#7460,.F.) ;
#10100 = ORIENTED_EDGE('',*,*,#7558,.T.) ;
#10101 = ORIENTED_EDGE('',*,*,#7461,.F.) ;
#10102 = ORIENTED_EDGE('',*,*,#7559,.F.) ;
#10103 = ORIENTED_EDGE('',*,*,#7462,.F.) ;
#10104 = ORIENTED_EDGE('',*,*,#7558,.F.) ;
#10105 = ORIENTED_EDGE('',*,*,#7459,.F.) ;
#10106 = ORIENTED_EDGE('',*,*,#7559,.T.) ;
#10107 = ORIENTED_EDGE('',*,*,#7464,.F.) ;
#10108 = ORIENTED_EDGE('',*,*,#7560,.T.) ;
#10109 = ORIENTED_EDGE('',*,*,#7465,.F.) ;
#10110 = ORIENTED_EDGE('',*,*,#7561,.F.) ;
#10111 = ORIENTED_EDGE('',*,*,#7562,.F.) ;
#10112 = ORIENTED_EDGE('',*,*,#7468,.F.) ;
#10113 = ORIENTED_EDGE('',*,*,#7466,.F.) ;
#10114 = ORIENTED_EDGE('',*,*,#7560,.F.) ;
#10115 = ORIENTED_EDGE('',*,*,#7463,.F.) ;
#10116 = ORIENTED_EDGE('',*,*,#7562,.T.) ;
#10117 = ORIENTED_EDGE('',*,*,#7563,.T.) ;
#10118 = ORIENTED_EDGE('',*,*,#7564,.F.) ;
#10119 = ORIENTED_EDGE('',*,*,#7565,.F.) ;
#10120 = ORIENTED_EDGE('',*,*,#7470,.F.) ;
#10121 = ORIENTED_EDGE('',*,*,#7566,.F.) ;
#10122 = ORIENTED_EDGE('',*,*,#7563,.F.) ;
#10123 = ORIENTED_EDGE('',*,*,#7561,.T.) ;
#10124 = ORIENTED_EDGE('',*,*,#7469,.F.) ;
#10125 = ORIENTED_EDGE('',*,*,#7565,.T.) ;
#10126 = ORIENTED_EDGE('',*,*,#7567,.T.) ;
#10127 = ORIENTED_EDGE('',*,*,#7568,.F.) ;
#10128 = ORIENTED_EDGE('',*,*,#7472,.F.) ;
#10129 = ORIENTED_EDGE('',*,*,#7569,.F.) ;
#10130 = ORIENTED_EDGE('',*,*,#7567,.F.) ;
#10131 = ORIENTED_EDGE('',*,*,#7564,.T.) ;
#10132 = ORIENTED_EDGE('',*,*,#7566,.T.) ;
#10133 = ORIENTED_EDGE('',*,*,#7471,.F.) ;
#10134 = ORIENTED_EDGE('',*,*,#7568,.T.) ;
#10135 = ORIENTED_EDGE('',*,*,#7570,.T.) ;
#10136 = ORIENTED_EDGE('',*,*,#7571,.F.) ;
#10137 = ORIENTED_EDGE('',*,*,#7572,.F.) ;
#10138 = ORIENTED_EDGE('',*,*,#7474,.F.) ;
#10139 = ORIENTED_EDGE('',*,*,#7573,.F.) ;
#10140 = ORIENTED_EDGE('',*,*,#7570,.F.) ;
#10141 = ORIENTED_EDGE('',*,*,#7569,.T.) ;
#10142 = ORIENTED_EDGE('',*,*,#7473,.F.) ;
#10143 = ORIENTED_EDGE('',*,*,#7572,.T.) ;
#10144 = ORIENTED_EDGE('',*,*,#7574,.T.) ;
#10145 = ORIENTED_EDGE('',*,*,#7575,.F.) ;
#10146 = ORIENTED_EDGE('',*,*,#7476,.F.) ;
#10147 = ORIENTED_EDGE('',*,*,#7576,.F.) ;
#10148 = ORIENTED_EDGE('',*,*,#7574,.F.) ;
#10149 = ORIENTED_EDGE('',*,*,#7571,.T.) ;
#10150 = ORIENTED_EDGE('',*,*,#7573,.T.) ;
#10151 = ORIENTED_EDGE('',*,*,#7475,.F.) ;
#10152 = ORIENTED_EDGE('',*,*,#7575,.T.) ;
#10153 = ORIENTED_EDGE('',*,*,#7576,.T.) ;
#10154 = ORIENTED_EDGE('',*,*,#7480,.F.) ;
#10155 = ORIENTED_EDGE('',*,*,#7478,.F.) ;
#10156 = ORIENTED_EDGE('',*,*,#7577,.T.) ;
#10157 = ORIENTED_EDGE('',*,*,#7481,.F.) ;
#10158 = ORIENTED_EDGE('',*,*,#7578,.F.) ;
#10159 = ORIENTED_EDGE('',*,*,#7482,.F.) ;
#10160 = ORIENTED_EDGE('',*,*,#7577,.F.) ;
#10161 = ORIENTED_EDGE('',*,*,#7477,.F.) ;
#10162 = ORIENTED_EDGE('',*,*,#7578,.T.) ;
#10163 = ORIENTED_EDGE('',*,*,#7484,.F.) ;
#10164 = ORIENTED_EDGE('',*,*,#7579,.T.) ;
#10165 = ORIENTED_EDGE('',*,*,#7485,.F.) ;
#10166 = ORIENTED_EDGE('',*,*,#7580,.F.) ;
#10167 = ORIENTED_EDGE('',*,*,#7486,.F.) ;
#10168 = ORIENTED_EDGE('',*,*,#7579,.F.) ;
#10169 = ORIENTED_EDGE('',*,*,#7483,.F.) ;
#10170 = ORIENTED_EDGE('',*,*,#7580,.T.) ;
#10171 = ORIENTED_EDGE('',*,*,#7488,.F.) ;
#10172 = ORIENTED_EDGE('',*,*,#7581,.T.) ;
#10173 = ORIENTED_EDGE('',*,*,#7489,.F.) ;
#10174 = ORIENTED_EDGE('',*,*,#7582,.F.) ;
#10175 = ORIENTED_EDGE('',*,*,#7490,.F.) ;
#10176 = ORIENTED_EDGE('',*,*,#7581,.F.) ;
#10177 = ORIENTED_EDGE('',*,*,#7487,.F.) ;
#10178 = ORIENTED_EDGE('',*,*,#7582,.T.) ;
#10179 = ORIENTED_EDGE('',*,*,#7492,.F.) ;
#10180 = ORIENTED_EDGE('',*,*,#7583,.T.) ;
#10181 = ORIENTED_EDGE('',*,*,#7493,.F.) ;
#10182 = ORIENTED_EDGE('',*,*,#7584,.F.) ;
#10183 = ORIENTED_EDGE('',*,*,#7585,.F.) ;
#10184 = ORIENTED_EDGE('',*,*,#7496,.F.) ;
#10185 = ORIENTED_EDGE('',*,*,#7494,.F.) ;
#10186 = ORIENTED_EDGE('',*,*,#7583,.F.) ;
#10187 = ORIENTED_EDGE('',*,*,#7491,.F.) ;
#10188 = ORIENTED_EDGE('',*,*,#7585,.T.) ;
#10189 = ORIENTED_EDGE('',*,*,#7586,.T.) ;
#10190 = ORIENTED_EDGE('',*,*,#7587,.F.) ;
#10191 = ORIENTED_EDGE('',*,*,#7588,.F.) ;
#10192 = ORIENTED_EDGE('',*,*,#7498,.F.) ;
#10193 = ORIENTED_EDGE('',*,*,#7589,.F.) ;
#10194 = ORIENTED_EDGE('',*,*,#7586,.F.) ;
#10195 = ORIENTED_EDGE('',*,*,#7584,.T.) ;
#10196 = ORIENTED_EDGE('',*,*,#7497,.F.) ;
#10197 = ORIENTED_EDGE('',*,*,#7588,.T.) ;
#10198 = ORIENTED_EDGE('',*,*,#7590,.T.) ;
#10199 = ORIENTED_EDGE('',*,*,#7591,.F.) ;
#10200 = ORIENTED_EDGE('',*,*,#7590,.F.) ;
#10201 = ORIENTED_EDGE('',*,*,#7587,.T.) ;
#10202 = ORIENTED_EDGE('',*,*,#7589,.T.) ;
#10203 = ORIENTED_EDGE('',*,*,#7499,.F.) ;
#10204 = ORIENTED_EDGE('',*,*,#7591,.T.) ;
#10205 = ORIENTED_EDGE('',*,*,#7592,.T.) ;
#10206 = ORIENTED_EDGE('',*,*,#7593,.T.) ;
#10207 = ORIENTED_EDGE('',*,*,#7593,.F.) ;
#10208 = ORIENTED_EDGE('',*,*,#7592,.F.) ;
#10209 = ORIENTED_EDGE('',*,*,#7594,.F.) ;
#10210 = ORIENTED_EDGE('',*,*,#7594,.T.) ;
#10211 = ORIENTED_EDGE('',*,*,#7595,.T.) ;
#10212 = ORIENTED_EDGE('',*,*,#7596,.F.) ;
#10213 = ORIENTED_EDGE('',*,*,#7596,.T.) ;
#10214 = ORIENTED_EDGE('',*,*,#7595,.F.) ;
#10215 = ORIENTED_EDGE('',*,*,#7597,.T.) ;
#10216 = ORIENTED_EDGE('',*,*,#7597,.F.) ;
#10217 = ORIENTED_EDGE('',*,*,#7598,.F.) ;
#10218 = ORIENTED_EDGE('',*,*,#7599,.F.) ;
#10219 = ORIENTED_EDGE('',*,*,#7599,.T.) ;
#10220 = ORIENTED_EDGE('',*,*,#7600,.T.) ;
#10221 = ORIENTED_EDGE('',*,*,#7598,.T.) ;
#10222 = ORIENTED_EDGE('',*,*,#7600,.F.) ;
#10223 = ORIENTED_EDGE('',*,*,#7601,.F.) ;
#10224 = ORIENTED_EDGE('',*,*,#7602,.F.) ;
#10225 = ORIENTED_EDGE('',*,*,#7602,.T.) ;
#10226 = ORIENTED_EDGE('',*,*,#7601,.T.) ;
#10227 = ORIENTED_EDGE('',*,*,#7603,.T.) ;
#10228 = ORIENTED_EDGE('',*,*,#7604,.F.) ;
#10229 = ORIENTED_EDGE('',*,*,#7605,.F.) ;
#10230 = ORIENTED_EDGE('',*,*,#7603,.F.) ;
#10231 = ORIENTED_EDGE('',*,*,#7605,.T.) ;
#10232 = ORIENTED_EDGE('',*,*,#7606,.T.) ;
#10233 = ORIENTED_EDGE('',*,*,#7604,.T.) ;
#10234 = ORIENTED_EDGE('',*,*,#7606,.F.) ;
#10235 = ORIENTED_EDGE('',*,*,#7607,.T.) ;
#10236 = ORIENTED_EDGE('',*,*,#7608,.T.) ;
#10237 = ORIENTED_EDGE('',*,*,#7609,.F.) ;
#10238 = ORIENTED_EDGE('',*,*,#7608,.F.) ;
#10239 = ORIENTED_EDGE('',*,*,#7609,.T.) ;
#10240 = ORIENTED_EDGE('',*,*,#7610,.T.) ;
#10241 = ORIENTED_EDGE('',*,*,#7610,.F.) ;
#10242 = ORIENTED_EDGE('',*,*,#7607,.F.) ;
#10243 = ORIENTED_EDGE('',*,*,#7611,.F.) ;
#10244 = ORIENTED_EDGE('',*,*,#7611,.T.) ;
#10245 = ORIENTED_EDGE('',*,*,#7612,.T.) ;
#10246 = ORIENTED_EDGE('',*,*,#7613,.F.) ;
#10247 = ORIENTED_EDGE('',*,*,#7613,.T.) ;
#10248 = ORIENTED_EDGE('',*,*,#7612,.F.) ;
#10249 = ORIENTED_EDGE('',*,*,#7614,.T.) ;
#10250 = ORIENTED_EDGE('',*,*,#7614,.F.) ;
#10251 = ORIENTED_EDGE('',*,*,#7615,.F.) ;
#10252 = ORIENTED_EDGE('',*,*,#7616,.F.) ;
#10253 = ORIENTED_EDGE('',*,*,#7616,.T.) ;
#10254 = ORIENTED_EDGE('',*,*,#7615,.T.) ;
#10255 = ORIENTED_EDGE('',*,*,#7617,.T.) ;
#10256 = ORIENTED_EDGE('',*,*,#7618,.F.) ;
#10257 = ORIENTED_EDGE('',*,*,#7617,.F.) ;
#10258 = ORIENTED_EDGE('',*,*,#7618,.T.) ;
#10259 = ORIENTED_EDGE('',*,*,#7619,.T.) ;
#10260 = ORIENTED_EDGE('',*,*,#7619,.F.) ;
#10261 = ORIENTED_EDGE('',*,*,#7620,.T.) ;
#10262 = ORIENTED_EDGE('',*,*,#7621,.T.) ;
#10263 = ORIENTED_EDGE('',*,*,#7622,.F.) ;
#10264 = ORIENTED_EDGE('',*,*,#7621,.F.) ;
#10265 = ORIENTED_EDGE('',*,*,#7622,.T.) ;
#10266 = ORIENTED_EDGE('',*,*,#7623,.T.) ;
#10267 = ORIENTED_EDGE('',*,*,#7623,.F.) ;
#10268 = ORIENTED_EDGE('',*,*,#7620,.F.) ;
#10269 = ORIENTED_EDGE('',*,*,#7624,.F.) ;
#10270 = ORIENTED_EDGE('',*,*,#7624,.T.) ;
#10271 = ORIENTED_EDGE('',*,*,#7625,.T.) ;
#10272 = ORIENTED_EDGE('',*,*,#7626,.F.) ;
#10273 = ORIENTED_EDGE('',*,*,#7626,.T.) ;
#10274 = ORIENTED_EDGE('',*,*,#7625,.F.) ;
#10275 = ORIENTED_EDGE('',*,*,#7627,.T.) ;
#10276 = ORIENTED_EDGE('',*,*,#7627,.F.) ;
#10277 = ORIENTED_EDGE('',*,*,#7628,.F.) ;
#10278 = ORIENTED_EDGE('',*,*,#7629,.F.) ;
#10279 = ORIENTED_EDGE('',*,*,#7629,.T.) ;
#10280 = ORIENTED_EDGE('',*,*,#7628,.T.) ;
#10281 = ORIENTED_EDGE('',*,*,#7630,.T.) ;
#10282 = ORIENTED_EDGE('',*,*,#7631,.F.) ;
#10283 = ORIENTED_EDGE('',*,*,#7630,.F.) ;
#10284 = ORIENTED_EDGE('',*,*,#7631,.T.) ;
#10285 = ORIENTED_EDGE('',*,*,#7632,.T.) ;
#10286 = ORIENTED_EDGE('',*,*,#7632,.F.) ;
#10287 = ORIENTED_EDGE('',*,*,#7633,.T.) ;
#10288 = ORIENTED_EDGE('',*,*,#7634,.T.) ;
#10289 = ORIENTED_EDGE('',*,*,#7635,.F.) ;
#10290 = ORIENTED_EDGE('',*,*,#7634,.F.) ;
#10291 = ORIENTED_EDGE('',*,*,#7635,.T.) ;
#10292 = ORIENTED_EDGE('',*,*,#7636,.T.) ;
#10293 = ORIENTED_EDGE('',*,*,#7636,.F.) ;
#10294 = ORIENTED_EDGE('',*,*,#7633,.F.) ;
#10295 = ORIENTED_EDGE('',*,*,#7637,.F.) ;
#10296 = ORIENTED_EDGE('',*,*,#7637,.T.) ;
#10297 = ORIENTED_EDGE('',*,*,#7638,.T.) ;
#10298 = ORIENTED_EDGE('',*,*,#7639,.F.) ;
#10299 = ORIENTED_EDGE('',*,*,#7639,.T.) ;
#10300 = ORIENTED_EDGE('',*,*,#7638,.F.) ;
#10301 = ORIENTED_EDGE('',*,*,#7640,.T.) ;
#10302 = ORIENTED_EDGE('',*,*,#7640,.F.) ;
#10303 = ORIENTED_EDGE('',*,*,#7641,.F.) ;
#10304 = ORIENTED_EDGE('',*,*,#7642,.F.) ;
#10305 = ORIENTED_EDGE('',*,*,#7642,.T.) ;
#10306 = ORIENTED_EDGE('',*,*,#7641,.T.) ;
#10307 = ORIENTED_EDGE('',*,*,#7643,.T.) ;
#10308 = ORIENTED_EDGE('',*,*,#7644,.F.) ;
#10309 = ORIENTED_EDGE('',*,*,#7643,.F.) ;
#10310 = ORIENTED_EDGE('',*,*,#7644,.T.) ;
#10311 = ORIENTED_EDGE('',*,*,#7645,.T.) ;
#10312 = ORIENTED_EDGE('',*,*,#7645,.F.) ;
#10313 = ORIENTED_EDGE('',*,*,#7646,.T.) ;
#10314 = ORIENTED_EDGE('',*,*,#7647,.T.) ;
#10315 = ORIENTED_EDGE('',*,*,#7648,.F.) ;
#10316 = ORIENTED_EDGE('',*,*,#7647,.F.) ;
#10317 = ORIENTED_EDGE('',*,*,#7648,.T.) ;
#10318 = ORIENTED_EDGE('',*,*,#7649,.T.) ;
#10319 = ORIENTED_EDGE('',*,*,#7649,.F.) ;
#10320 = ORIENTED_EDGE('',*,*,#7646,.F.) ;
#10321 = ORIENTED_EDGE('',*,*,#7650,.T.) ;
#10322 = ORIENTED_EDGE('',*,*,#7650,.F.) ;
#10323 = ORIENTED_EDGE('',*,*,#7651,.F.) ;
#10324 = ORIENTED_EDGE('',*,*,#7651,.T.) ;
#10325 = ORIENTED_EDGE('',*,*,#7652,.T.) ;
#10326 = ORIENTED_EDGE('',*,*,#7653,.F.) ;
#10327 = ORIENTED_EDGE('',*,*,#7652,.F.) ;
#10328 = ORIENTED_EDGE('',*,*,#7653,.T.) ;
#10329 = ORIENTED_EDGE('',*,*,#7654,.F.) ;
#10330 = ORIENTED_EDGE('',*,*,#7655,.F.) ;
#10331 = ORIENTED_EDGE('',*,*,#7655,.T.) ;
#10332 = ORIENTED_EDGE('',*,*,#7656,.T.) ;
#10333 = ORIENTED_EDGE('',*,*,#7654,.T.) ;
#10334 = ORIENTED_EDGE('',*,*,#7656,.F.) ;
#10335 = ORIENTED_EDGE('',*,*,#7657,.T.) ;
#10336 = ORIENTED_EDGE('',*,*,#7657,.F.) ;
#10337 = ORIENTED_EDGE('',*,*,#7658,.F.) ;
#10338 = ORIENTED_EDGE('',*,*,#7659,.F.) ;
#10339 = ORIENTED_EDGE('',*,*,#7660,.F.) ;
#10340 = ORIENTED_EDGE('',*,*,#7660,.T.) ;
#10341 = ORIENTED_EDGE('',*,*,#7661,.F.) ;
#10342 = ORIENTED_EDGE('',*,*,#7662,.T.) ;
#10343 = ORIENTED_EDGE('',*,*,#7662,.F.) ;
#10344 = ORIENTED_EDGE('',*,*,#7658,.T.) ;
#10345 = ORIENTED_EDGE('',*,*,#7659,.T.) ;
#10346 = ORIENTED_EDGE('',*,*,#7661,.T.) ;
#10347 = ORIENTED_EDGE('',*,*,#7663,.F.) ;
#10348 = ORIENTED_EDGE('',*,*,#7664,.F.) ;
#10349 = ORIENTED_EDGE('',*,*,#7664,.T.) ;
#10350 = ORIENTED_EDGE('',*,*,#7665,.F.) ;
#10351 = ORIENTED_EDGE('',*,*,#7666,.T.) ;
#10352 = ORIENTED_EDGE('',*,*,#7666,.F.) ;
#10353 = ORIENTED_EDGE('',*,*,#7667,.T.) ;
#10354 = ORIENTED_EDGE('',*,*,#7663,.T.) ;
#10355 = ORIENTED_EDGE('',*,*,#7665,.T.) ;
#10356 = ORIENTED_EDGE('',*,*,#7667,.F.) ;
#10357 = ORIENTED_EDGE('',*,*,#7668,.T.) ;
#10358 = ORIENTED_EDGE('',*,*,#7668,.F.) ;
#10359 = ORIENTED_EDGE('',*,*,#7669,.F.) ;
#10360 = ORIENTED_EDGE('',*,*,#7670,.F.) ;
#10361 = ORIENTED_EDGE('',*,*,#7670,.T.) ;
#10362 = ORIENTED_EDGE('',*,*,#7671,.T.) ;
#10363 = ORIENTED_EDGE('',*,*,#7669,.T.) ;
#10364 = ORIENTED_EDGE('',*,*,#7671,.F.) ;
#10365 = ORIENTED_EDGE('',*,*,#7672,.F.) ;
#10366 = ORIENTED_EDGE('',*,*,#7672,.T.) ;
#10367 = ORIENTED_EDGE('',*,*,#7673,.T.) ;
#10368 = ORIENTED_EDGE('',*,*,#7674,.T.) ;
#10369 = ORIENTED_EDGE('',*,*,#7673,.F.) ;
#10370 = ORIENTED_EDGE('',*,*,#7675,.F.) ;
#10371 = ORIENTED_EDGE('',*,*,#7675,.T.) ;
#10372 = ORIENTED_EDGE('',*,*,#7674,.F.) ;
#10373 = ORIENTED_EDGE('',*,*,#7676,.T.) ;
#10374 = ORIENTED_EDGE('',*,*,#7676,.F.) ;
#10375 = ORIENTED_EDGE('',*,*,#7677,.F.) ;
#10376 = ORIENTED_EDGE('',*,*,#7678,.T.) ;
#10377 = ORIENTED_EDGE('',*,*,#7679,.F.) ;
#10378 = ORIENTED_EDGE('',*,*,#7680,.F.) ;
#10379 = ORIENTED_EDGE('',*,*,#7680,.T.) ;
#10380 = ORIENTED_EDGE('',*,*,#7681,.F.) ;
#10381 = ORIENTED_EDGE('',*,*,#7682,.T.) ;
#10382 = ORIENTED_EDGE('',*,*,#7682,.F.) ;
#10383 = ORIENTED_EDGE('',*,*,#7677,.T.) ;
#10384 = ORIENTED_EDGE('',*,*,#7683,.F.) ;
#10385 = ORIENTED_EDGE('',*,*,#7683,.T.) ;
#10386 = ORIENTED_EDGE('',*,*,#7678,.F.) ;
#10387 = ORIENTED_EDGE('',*,*,#7679,.T.) ;
#10388 = ORIENTED_EDGE('',*,*,#7681,.T.) ;
#10389 = ORIENTED_EDGE('',*,*,#7684,.T.) ;
#10390 = ORIENTED_EDGE('',*,*,#7685,.T.) ;
#10391 = ORIENTED_EDGE('',*,*,#7686,.T.) ;
#10392 = ORIENTED_EDGE('',*,*,#7687,.T.) ;
#10393 = ORIENTED_EDGE('',*,*,#7688,.T.) ;
#10394 = ORIENTED_EDGE('',*,*,#7689,.T.) ;
#10395 = ORIENTED_EDGE('',*,*,#7690,.T.) ;
#10396 = ORIENTED_EDGE('',*,*,#7691,.T.) ;
#10397 = ORIENTED_EDGE('',*,*,#7692,.T.) ;
#10398 = ORIENTED_EDGE('',*,*,#7693,.T.) ;
#10399 = ORIENTED_EDGE('',*,*,#7694,.T.) ;
#10400 = ORIENTED_EDGE('',*,*,#7695,.T.) ;
#10401 = ORIENTED_EDGE('',*,*,#7696,.T.) ;
#10402 = ORIENTED_EDGE('',*,*,#7697,.T.) ;
#10403 = ORIENTED_EDGE('',*,*,#7698,.T.) ;
#10404 = ORIENTED_EDGE('',*,*,#7699,.T.) ;
#10405 = ORIENTED_EDGE('',*,*,#7700,.T.) ;
#10406 = ORIENTED_EDGE('',*,*,#7701,.T.) ;
#10407 = ORIENTED_EDGE('',*,*,#7702,.T.) ;
#10408 = ORIENTED_EDGE('',*,*,#7703,.T.) ;
#10409 = ORIENTED_EDGE('',*,*,#7704,.T.) ;
#10410 = ORIENTED_EDGE('',*,*,#7705,.T.) ;
#10411 = ORIENTED_EDGE('',*,*,#7706,.T.) ;
#10412 = ORIENTED_EDGE('',*,*,#7707,.T.) ;
#10413 = ORIENTED_EDGE('',*,*,#7708,.T.) ;
#10414 = ORIENTED_EDGE('',*,*,#7709,.F.) ;
#10415 = ORIENTED_EDGE('',*,*,#7710,.T.) ;
#10416 = ORIENTED_EDGE('',*,*,#7711,.F.) ;
#10417 = ORIENTED_EDGE('',*,*,#7711,.T.) ;
#10418 = ORIENTED_EDGE('',*,*,#7712,.T.) ;
#10419 = ORIENTED_EDGE('',*,*,#7713,.T.) ;
#10420 = ORIENTED_EDGE('',*,*,#7714,.F.) ;
#10421 = ORIENTED_EDGE('',*,*,#7715,.T.) ;
#10422 = ORIENTED_EDGE('',*,*,#7716,.T.) ;
#10423 = ORIENTED_EDGE('',*,*,#7709,.T.) ;
#10424 = ORIENTED_EDGE('',*,*,#7717,.T.) ;
#10425 = ORIENTED_EDGE('',*,*,#7715,.F.) ;
#10426 = ORIENTED_EDGE('',*,*,#7718,.F.) ;
#10427 = ORIENTED_EDGE('',*,*,#7719,.T.) ;
#10428 = ORIENTED_EDGE('',*,*,#7720,.F.) ;
#10429 = ORIENTED_EDGE('',*,*,#7721,.F.) ;
#10430 = ORIENTED_EDGE('',*,*,#7722,.F.) ;
#10431 = ORIENTED_EDGE('',*,*,#7723,.F.) ;
#10432 = ORIENTED_EDGE('',*,*,#7719,.F.) ;
#10433 = ORIENTED_EDGE('',*,*,#7718,.T.) ;
#10434 = ORIENTED_EDGE('',*,*,#7724,.T.) ;
#10435 = ORIENTED_EDGE('',*,*,#7720,.T.) ;
#10436 = ORIENTED_EDGE('',*,*,#7723,.T.) ;
#10437 = ORIENTED_EDGE('',*,*,#7725,.T.) ;
#10438 = ORIENTED_EDGE('',*,*,#7726,.F.) ;
#10439 = ORIENTED_EDGE('',*,*,#7727,.F.) ;
#10440 = ORIENTED_EDGE('',*,*,#7728,.F.) ;
#10441 = ORIENTED_EDGE('',*,*,#7725,.F.) ;
#10442 = ORIENTED_EDGE('',*,*,#7729,.F.) ;
#10443 = ORIENTED_EDGE('',*,*,#7730,.T.) ;
#10444 = ORIENTED_EDGE('',*,*,#7731,.T.) ;
#10445 = ORIENTED_EDGE('',*,*,#7732,.F.) ;
#10446 = ORIENTED_EDGE('',*,*,#7726,.T.) ;
#10447 = ORIENTED_EDGE('',*,*,#7728,.T.) ;
#10448 = ORIENTED_EDGE('',*,*,#7733,.F.) ;
#10449 = ORIENTED_EDGE('',*,*,#7734,.T.) ;
#10450 = ORIENTED_EDGE('',*,*,#7684,.F.) ;
#10451 = ORIENTED_EDGE('',*,*,#7735,.F.) ;
#10452 = ORIENTED_EDGE('',*,*,#7685,.F.) ;
#10453 = ORIENTED_EDGE('',*,*,#7734,.F.) ;
#10454 = ORIENTED_EDGE('',*,*,#7736,.F.) ;
#10455 = ORIENTED_EDGE('',*,*,#7735,.T.) ;
#10456 = ORIENTED_EDGE('',*,*,#7687,.F.) ;
#10457 = ORIENTED_EDGE('',*,*,#7737,.T.) ;
#10458 = ORIENTED_EDGE('',*,*,#7688,.F.) ;
#10459 = ORIENTED_EDGE('',*,*,#7738,.F.) ;
#10460 = ORIENTED_EDGE('',*,*,#7689,.F.) ;
#10461 = ORIENTED_EDGE('',*,*,#7737,.F.) ;
#10462 = ORIENTED_EDGE('',*,*,#7686,.F.) ;
#10463 = ORIENTED_EDGE('',*,*,#7738,.T.) ;
#10464 = ORIENTED_EDGE('',*,*,#7691,.F.) ;
#10465 = ORIENTED_EDGE('',*,*,#7739,.T.) ;
#10466 = ORIENTED_EDGE('',*,*,#7740,.F.) ;
#10467 = ORIENTED_EDGE('',*,*,#7741,.F.) ;
#10468 = ORIENTED_EDGE('',*,*,#7742,.F.) ;
#10469 = ORIENTED_EDGE('',*,*,#7739,.F.) ;
#10470 = ORIENTED_EDGE('',*,*,#7690,.F.) ;
#10471 = ORIENTED_EDGE('',*,*,#7741,.T.) ;
#10472 = ORIENTED_EDGE('',*,*,#7743,.F.) ;
#10473 = ORIENTED_EDGE('',*,*,#7744,.T.) ;
#10474 = ORIENTED_EDGE('',*,*,#7745,.F.) ;
#10475 = ORIENTED_EDGE('',*,*,#7746,.F.) ;
#10476 = ORIENTED_EDGE('',*,*,#7747,.F.) ;
#10477 = ORIENTED_EDGE('',*,*,#7744,.F.) ;
#10478 = ORIENTED_EDGE('',*,*,#7748,.F.) ;
#10479 = ORIENTED_EDGE('',*,*,#7746,.T.) ;
#10480 = ORIENTED_EDGE('',*,*,#7749,.F.) ;
#10481 = ORIENTED_EDGE('',*,*,#7750,.T.) ;
#10482 = ORIENTED_EDGE('',*,*,#7692,.F.) ;
#10483 = ORIENTED_EDGE('',*,*,#7751,.F.) ;
#10484 = ORIENTED_EDGE('',*,*,#7693,.F.) ;
#10485 = ORIENTED_EDGE('',*,*,#7750,.F.) ;
#10486 = ORIENTED_EDGE('',*,*,#7752,.F.) ;
#10487 = ORIENTED_EDGE('',*,*,#7751,.T.) ;
#10488 = ORIENTED_EDGE('',*,*,#7695,.F.) ;
#10489 = ORIENTED_EDGE('',*,*,#7753,.T.) ;
#10490 = ORIENTED_EDGE('',*,*,#7696,.F.) ;
#10491 = ORIENTED_EDGE('',*,*,#7754,.F.) ;
#10492 = ORIENTED_EDGE('',*,*,#7697,.F.) ;
#10493 = ORIENTED_EDGE('',*,*,#7753,.F.) ;
#10494 = ORIENTED_EDGE('',*,*,#7694,.F.) ;
#10495 = ORIENTED_EDGE('',*,*,#7754,.T.) ;
#10496 = ORIENTED_EDGE('',*,*,#7699,.F.) ;
#10497 = ORIENTED_EDGE('',*,*,#7755,.T.) ;
#10498 = ORIENTED_EDGE('',*,*,#7756,.F.) ;
#10499 = ORIENTED_EDGE('',*,*,#7757,.F.) ;
#10500 = ORIENTED_EDGE('',*,*,#7758,.F.) ;
#10501 = ORIENTED_EDGE('',*,*,#7755,.F.) ;
#10502 = ORIENTED_EDGE('',*,*,#7698,.F.) ;
#10503 = ORIENTED_EDGE('',*,*,#7757,.T.) ;
#10504 = ORIENTED_EDGE('',*,*,#7759,.F.) ;
#10505 = ORIENTED_EDGE('',*,*,#7760,.T.) ;
#10506 = ORIENTED_EDGE('',*,*,#7761,.F.) ;
#10507 = ORIENTED_EDGE('',*,*,#7762,.F.) ;
#10508 = ORIENTED_EDGE('',*,*,#7763,.F.) ;
#10509 = ORIENTED_EDGE('',*,*,#7760,.F.) ;
#10510 = ORIENTED_EDGE('',*,*,#7764,.F.) ;
#10511 = ORIENTED_EDGE('',*,*,#7762,.T.) ;
#10512 = ORIENTED_EDGE('',*,*,#7765,.F.) ;
#10513 = ORIENTED_EDGE('',*,*,#7766,.T.) ;
#10514 = ORIENTED_EDGE('',*,*,#7700,.F.) ;
#10515 = ORIENTED_EDGE('',*,*,#7767,.F.) ;
#10516 = ORIENTED_EDGE('',*,*,#7701,.F.) ;
#10517 = ORIENTED_EDGE('',*,*,#7766,.F.) ;
#10518 = ORIENTED_EDGE('',*,*,#7768,.F.) ;
#10519 = ORIENTED_EDGE('',*,*,#7767,.T.) ;
#10520 = ORIENTED_EDGE('',*,*,#7703,.F.) ;
#10521 = ORIENTED_EDGE('',*,*,#7769,.T.) ;
#10522 = ORIENTED_EDGE('',*,*,#7704,.F.) ;
#10523 = ORIENTED_EDGE('',*,*,#7770,.F.) ;
#10524 = ORIENTED_EDGE('',*,*,#7705,.F.) ;
#10525 = ORIENTED_EDGE('',*,*,#7769,.F.) ;
#10526 = ORIENTED_EDGE('',*,*,#7702,.F.) ;
#10527 = ORIENTED_EDGE('',*,*,#7770,.T.) ;
#10528 = ORIENTED_EDGE('',*,*,#7707,.F.) ;
#10529 = ORIENTED_EDGE('',*,*,#7771,.T.) ;
#10530 = ORIENTED_EDGE('',*,*,#7772,.F.) ;
#10531 = ORIENTED_EDGE('',*,*,#7773,.F.) ;
#10532 = ORIENTED_EDGE('',*,*,#7774,.F.) ;
#10533 = ORIENTED_EDGE('',*,*,#7771,.F.) ;
#10534 = ORIENTED_EDGE('',*,*,#7706,.F.) ;
#10535 = ORIENTED_EDGE('',*,*,#7773,.T.) ;
#10536 = ORIENTED_EDGE('',*,*,#7775,.F.) ;
#10537 = ORIENTED_EDGE('',*,*,#7776,.T.) ;
#10538 = ORIENTED_EDGE('',*,*,#7777,.F.) ;
#10539 = ORIENTED_EDGE('',*,*,#7778,.F.) ;
#10540 = ORIENTED_EDGE('',*,*,#7779,.F.) ;
#10541 = ORIENTED_EDGE('',*,*,#7776,.F.) ;
#10542 = ORIENTED_EDGE('',*,*,#7780,.F.) ;
#10543 = ORIENTED_EDGE('',*,*,#7778,.T.) ;
#10544 = ORIENTED_EDGE('',*,*,#7781,.F.) ;
#10545 = ORIENTED_EDGE('',*,*,#7782,.T.) ;
#10546 = ORIENTED_EDGE('',*,*,#7712,.F.) ;
#10547 = ORIENTED_EDGE('',*,*,#7710,.F.) ;
#10548 = ORIENTED_EDGE('',*,*,#7783,.F.) ;
#10549 = ORIENTED_EDGE('',*,*,#7784,.F.) ;
#10550 = ORIENTED_EDGE('',*,*,#7782,.F.) ;
#10551 = ORIENTED_EDGE('',*,*,#7785,.F.) ;
#10552 = ORIENTED_EDGE('',*,*,#7717,.F.) ;
#10553 = ORIENTED_EDGE('',*,*,#7708,.F.) ;
#10554 = ORIENTED_EDGE('',*,*,#7716,.F.) ;
#10555 = ORIENTED_EDGE('',*,*,#7784,.T.) ;
#10556 = ORIENTED_EDGE('',*,*,#7786,.T.) ;
#10557 = ORIENTED_EDGE('',*,*,#7787,.F.) ;
#10558 = ORIENTED_EDGE('',*,*,#7786,.F.) ;
#10559 = ORIENTED_EDGE('',*,*,#7783,.T.) ;
#10560 = ORIENTED_EDGE('',*,*,#7713,.F.) ;
#10561 = ORIENTED_EDGE('',*,*,#7787,.T.) ;
#10562 = ORIENTED_EDGE('',*,*,#7714,.T.) ;
#10563 = ORIENTED_EDGE('',*,*,#7785,.T.) ;
#10564 = ORIENTED_EDGE('',*,*,#7781,.T.) ;
#10565 = ORIENTED_EDGE('',*,*,#7777,.T.) ;
#10566 = ORIENTED_EDGE('',*,*,#7779,.T.) ;
#10567 = ORIENTED_EDGE('',*,*,#7780,.T.) ;
#10568 = ORIENTED_EDGE('',*,*,#7775,.T.) ;
#10569 = ORIENTED_EDGE('',*,*,#7772,.T.) ;
#10570 = ORIENTED_EDGE('',*,*,#7774,.T.) ;
#10571 = ORIENTED_EDGE('',*,*,#7768,.T.) ;
#10572 = ORIENTED_EDGE('',*,*,#7765,.T.) ;
#10573 = ORIENTED_EDGE('',*,*,#7761,.T.) ;
#10574 = ORIENTED_EDGE('',*,*,#7763,.T.) ;
#10575 = ORIENTED_EDGE('',*,*,#7764,.T.) ;
#10576 = ORIENTED_EDGE('',*,*,#7759,.T.) ;
#10577 = ORIENTED_EDGE('',*,*,#7756,.T.) ;
#10578 = ORIENTED_EDGE('',*,*,#7758,.T.) ;
#10579 = ORIENTED_EDGE('',*,*,#7752,.T.) ;
#10580 = ORIENTED_EDGE('',*,*,#7749,.T.) ;
#10581 = ORIENTED_EDGE('',*,*,#7745,.T.) ;
#10582 = ORIENTED_EDGE('',*,*,#7747,.T.) ;
#10583 = ORIENTED_EDGE('',*,*,#7748,.T.) ;
#10584 = ORIENTED_EDGE('',*,*,#7743,.T.) ;
#10585 = ORIENTED_EDGE('',*,*,#7740,.T.) ;
#10586 = ORIENTED_EDGE('',*,*,#7742,.T.) ;
#10587 = ORIENTED_EDGE('',*,*,#7736,.T.) ;
#10588 = ORIENTED_EDGE('',*,*,#7788,.T.) ;
#10589 = ORIENTED_EDGE('',*,*,#7788,.F.) ;
#10590 = ORIENTED_EDGE('',*,*,#7733,.T.) ;
#10591 = ORIENTED_EDGE('',*,*,#7727,.T.) ;
#10592 = ORIENTED_EDGE('',*,*,#7789,.T.) ;
#10593 = ORIENTED_EDGE('',*,*,#7731,.F.) ;
#10594 = ORIENTED_EDGE('',*,*,#7790,.T.) ;
#10595 = ORIENTED_EDGE('',*,*,#7724,.F.) ;
#10596 = ORIENTED_EDGE('',*,*,#7790,.F.) ;
#10597 = ORIENTED_EDGE('',*,*,#7730,.F.) ;
#10598 = ORIENTED_EDGE('',*,*,#7729,.T.) ;
#10599 = ORIENTED_EDGE('',*,*,#7722,.T.) ;
#10600 = ORIENTED_EDGE('',*,*,#7791,.F.) ;
#10601 = ORIENTED_EDGE('',*,*,#7791,.T.) ;
#10602 = ORIENTED_EDGE('',*,*,#7721,.T.) ;
#10603 = ORIENTED_EDGE('',*,*,#7732,.T.) ;
#10604 = ORIENTED_EDGE('',*,*,#7789,.F.) ;
#10605 = ORIENTED_EDGE('',*,*,#7792,.F.) ;
#10606 = ORIENTED_EDGE('',*,*,#7792,.T.) ;
#10607 = ORIENTED_EDGE('',*,*,#7793,.F.) ;
#10608 = ORIENTED_EDGE('',*,*,#7793,.T.) ;
#10609 = ORIENTED_EDGE('',*,*,#7794,.F.) ;
#10610 = ORIENTED_EDGE('',*,*,#7795,.T.) ;
#10611 = ORIENTED_EDGE('',*,*,#7795,.F.) ;
#10612 = ORIENTED_EDGE('',*,*,#7794,.T.) ;
#10613 = ORIENTED_EDGE('',*,*,#7796,.F.) ;
#10614 = ORIENTED_EDGE('',*,*,#7796,.T.) ;
#10615 = ORIENTED_EDGE('',*,*,#7797,.F.) ;
#10616 = ORIENTED_EDGE('',*,*,#7798,.T.) ;
#10617 = ORIENTED_EDGE('',*,*,#7798,.F.) ;
#10618 = ORIENTED_EDGE('',*,*,#7797,.T.) ;
#10619 = ORIENTED_EDGE('',*,*,#7799,.F.) ;
#10620 = ORIENTED_EDGE('',*,*,#7799,.T.) ;
#10621 = ORIENTED_EDGE('',*,*,#7800,.F.) ;
#10622 = ORIENTED_EDGE('',*,*,#7801,.T.) ;
#10623 = ORIENTED_EDGE('',*,*,#7801,.F.) ;
#10624 = ORIENTED_EDGE('',*,*,#7800,.T.) ;
#10625 = ORIENTED_EDGE('',*,*,#7802,.F.) ;
#10626 = ORIENTED_EDGE('',*,*,#7802,.T.) ;
#10627 = ORIENTED_EDGE('',*,*,#7803,.F.) ;
#10628 = ORIENTED_EDGE('',*,*,#7804,.T.) ;
#10629 = ORIENTED_EDGE('',*,*,#7804,.F.) ;
#10630 = ORIENTED_EDGE('',*,*,#7803,.T.) ;
#10631 = ORIENTED_EDGE('',*,*,#7805,.F.) ;
#10632 = ORIENTED_EDGE('',*,*,#7805,.T.) ;
#10633 = ORIENTED_EDGE('',*,*,#7806,.F.) ;
#10634 = ORIENTED_EDGE('',*,*,#7807,.F.) ;
#10635 = ORIENTED_EDGE('',*,*,#7808,.F.) ;
#10636 = ORIENTED_EDGE('',*,*,#7809,.T.) ;
#10637 = ORIENTED_EDGE('',*,*,#7810,.F.) ;
#10638 = ORIENTED_EDGE('',*,*,#7809,.F.) ;
#10639 = ORIENTED_EDGE('',*,*,#7811,.F.) ;
#10640 = ORIENTED_EDGE('',*,*,#7812,.T.) ;
#10641 = ORIENTED_EDGE('',*,*,#7813,.F.) ;
#10642 = ORIENTED_EDGE('',*,*,#7812,.F.) ;
#10643 = ORIENTED_EDGE('',*,*,#7814,.F.) ;
#10644 = ORIENTED_EDGE('',*,*,#7815,.T.) ;
#10645 = ORIENTED_EDGE('',*,*,#7816,.F.) ;
#10646 = ORIENTED_EDGE('',*,*,#7815,.F.) ;
#10647 = ORIENTED_EDGE('',*,*,#7817,.F.) ;
#10648 = ORIENTED_EDGE('',*,*,#7807,.T.) ;
#10649 = ORIENTED_EDGE('',*,*,#7818,.F.) ;
#10650 = ORIENTED_EDGE('',*,*,#7819,.T.) ;
#10651 = ORIENTED_EDGE('',*,*,#7820,.F.) ;
#10652 = ORIENTED_EDGE('',*,*,#7819,.F.) ;
#10653 = ORIENTED_EDGE('',*,*,#7821,.F.) ;
#10654 = ORIENTED_EDGE('',*,*,#7822,.F.) ;
#10655 = ORIENTED_EDGE('',*,*,#7823,.F.) ;
#10656 = ORIENTED_EDGE('',*,*,#7824,.T.) ;
#10657 = ORIENTED_EDGE('',*,*,#7825,.F.) ;
#10658 = ORIENTED_EDGE('',*,*,#7824,.F.) ;
#10659 = ORIENTED_EDGE('',*,*,#7826,.F.) ;
#10660 = ORIENTED_EDGE('',*,*,#7827,.T.) ;
#10661 = ORIENTED_EDGE('',*,*,#7828,.F.) ;
#10662 = ORIENTED_EDGE('',*,*,#7827,.F.) ;
#10663 = ORIENTED_EDGE('',*,*,#7829,.F.) ;
#10664 = ORIENTED_EDGE('',*,*,#7830,.T.) ;
#10665 = ORIENTED_EDGE('',*,*,#7831,.F.) ;
#10666 = ORIENTED_EDGE('',*,*,#7830,.F.) ;
#10667 = ORIENTED_EDGE('',*,*,#7832,.F.) ;
#10668 = ORIENTED_EDGE('',*,*,#7822,.T.) ;
#10669 = ORIENTED_EDGE('',*,*,#7833,.F.) ;
#10670 = ORIENTED_EDGE('',*,*,#7834,.T.) ;
#10671 = ORIENTED_EDGE('',*,*,#7835,.F.) ;
#10672 = ORIENTED_EDGE('',*,*,#7834,.F.) ;
#10673 = ORIENTED_EDGE('',*,*,#7836,.F.) ;
#10674 = ORIENTED_EDGE('',*,*,#7837,.T.) ;
#10675 = ORIENTED_EDGE('',*,*,#7838,.T.) ;
#10676 = ORIENTED_EDGE('',*,*,#7839,.T.) ;
#10677 = ORIENTED_EDGE('',*,*,#7813,.T.) ;
#10678 = ORIENTED_EDGE('',*,*,#7816,.T.) ;
#10679 = ORIENTED_EDGE('',*,*,#7806,.T.) ;
#10680 = ORIENTED_EDGE('',*,*,#7810,.T.) ;
#10681 = ORIENTED_EDGE('',*,*,#7828,.T.) ;
#10682 = ORIENTED_EDGE('',*,*,#7831,.T.) ;
#10683 = ORIENTED_EDGE('',*,*,#7821,.T.) ;
#10684 = ORIENTED_EDGE('',*,*,#7825,.T.) ;
#10685 = ORIENTED_EDGE('',*,*,#7840,.T.) ;
#10686 = ORIENTED_EDGE('',*,*,#7838,.F.) ;
#10687 = ORIENTED_EDGE('',*,*,#7841,.F.) ;
#10688 = ORIENTED_EDGE('',*,*,#7842,.F.) ;
#10689 = ORIENTED_EDGE('',*,*,#7836,.T.) ;
#10690 = ORIENTED_EDGE('',*,*,#7843,.T.) ;
#10691 = ORIENTED_EDGE('',*,*,#7844,.F.) ;
#10692 = ORIENTED_EDGE('',*,*,#7845,.F.) ;
#10693 = ORIENTED_EDGE('',*,*,#7820,.T.) ;
#10694 = ORIENTED_EDGE('',*,*,#7835,.T.) ;
#10695 = ORIENTED_EDGE('',*,*,#7846,.T.) ;
#10696 = ORIENTED_EDGE('',*,*,#7847,.F.) ;
#10697 = ORIENTED_EDGE('',*,*,#7843,.F.) ;
#10698 = ORIENTED_EDGE('',*,*,#7839,.F.) ;
#10699 = ORIENTED_EDGE('',*,*,#7840,.F.) ;
#10700 = ORIENTED_EDGE('',*,*,#7848,.F.) ;
#10701 = ORIENTED_EDGE('',*,*,#7848,.T.) ;
#10702 = ORIENTED_EDGE('',*,*,#7842,.T.) ;
#10703 = ORIENTED_EDGE('',*,*,#7849,.T.) ;
#10704 = ORIENTED_EDGE('',*,*,#7850,.T.) ;
#10705 = ORIENTED_EDGE('',*,*,#7814,.T.) ;
#10706 = ORIENTED_EDGE('',*,*,#7811,.T.) ;
#10707 = ORIENTED_EDGE('',*,*,#7808,.T.) ;
#10708 = ORIENTED_EDGE('',*,*,#7817,.T.) ;
#10709 = ORIENTED_EDGE('',*,*,#7829,.T.) ;
#10710 = ORIENTED_EDGE('',*,*,#7826,.T.) ;
#10711 = ORIENTED_EDGE('',*,*,#7823,.T.) ;
#10712 = ORIENTED_EDGE('',*,*,#7832,.T.) ;
#10713 = ORIENTED_EDGE('',*,*,#7847,.T.) ;
#10714 = ORIENTED_EDGE('',*,*,#7851,.T.) ;
#10715 = ORIENTED_EDGE('',*,*,#7852,.T.) ;
#10716 = ORIENTED_EDGE('',*,*,#7844,.T.) ;
#10717 = ORIENTED_EDGE('',*,*,#7853,.T.) ;
#10718 = ORIENTED_EDGE('',*,*,#7851,.F.) ;
#10719 = ORIENTED_EDGE('',*,*,#7846,.F.) ;
#10720 = ORIENTED_EDGE('',*,*,#7850,.F.) ;
#10721 = ORIENTED_EDGE('',*,*,#7818,.T.) ;
#10722 = ORIENTED_EDGE('',*,*,#7833,.T.) ;
#10723 = ORIENTED_EDGE('',*,*,#7845,.T.) ;
#10724 = ORIENTED_EDGE('',*,*,#7852,.F.) ;
#10725 = ORIENTED_EDGE('',*,*,#7853,.F.) ;
#10726 = ORIENTED_EDGE('',*,*,#7849,.F.) ;
#10727 = ORIENTED_EDGE('',*,*,#7841,.T.) ;
#10728 = ORIENTED_EDGE('',*,*,#7837,.F.) ;
#10729 = ORIENTED_EDGE('',*,*,#7854,.F.) ;
#10730 = ORIENTED_EDGE('',*,*,#7855,.T.) ;
#10731 = ORIENTED_EDGE('',*,*,#7856,.T.) ;
#10732 = ORIENTED_EDGE('',*,*,#7857,.F.) ;
#10733 = ORIENTED_EDGE('',*,*,#7858,.F.) ;
#10734 = ORIENTED_EDGE('',*,*,#7859,.F.) ;
#10735 = ORIENTED_EDGE('',*,*,#7860,.F.) ;
#10736 = ORIENTED_EDGE('',*,*,#7861,.T.) ;
#10737 = ORIENTED_EDGE('',*,*,#7862,.T.) ;
#10738 = ORIENTED_EDGE('',*,*,#7863,.F.) ;
#10739 = ORIENTED_EDGE('',*,*,#7856,.F.) ;
#10740 = ORIENTED_EDGE('',*,*,#7855,.F.) ;
#10741 = ORIENTED_EDGE('',*,*,#7864,.F.) ;
#10742 = ORIENTED_EDGE('',*,*,#7865,.T.) ;
#10743 = ORIENTED_EDGE('',*,*,#7866,.T.) ;
#10744 = ORIENTED_EDGE('',*,*,#7867,.F.) ;
#10745 = ORIENTED_EDGE('',*,*,#7862,.F.) ;
#10746 = ORIENTED_EDGE('',*,*,#7861,.F.) ;
#10747 = ORIENTED_EDGE('',*,*,#7868,.F.) ;
#10748 = ORIENTED_EDGE('',*,*,#7859,.T.) ;
#10749 = ORIENTED_EDGE('',*,*,#7858,.T.) ;
#10750 = ORIENTED_EDGE('',*,*,#7869,.F.) ;
#10751 = ORIENTED_EDGE('',*,*,#7866,.F.) ;
#10752 = ORIENTED_EDGE('',*,*,#7865,.F.) ;
#10753 = ORIENTED_EDGE('',*,*,#7870,.F.) ;
#10754 = ORIENTED_EDGE('',*,*,#7871,.F.) ;
#10755 = ORIENTED_EDGE('',*,*,#7872,.F.) ;
#10756 = ORIENTED_EDGE('',*,*,#7873,.F.) ;
#10757 = ORIENTED_EDGE('',*,*,#7857,.T.) ;
#10758 = ORIENTED_EDGE('',*,*,#7863,.T.) ;
#10759 = ORIENTED_EDGE('',*,*,#7867,.T.) ;
#10760 = ORIENTED_EDGE('',*,*,#7869,.T.) ;
#10761 = ORIENTED_EDGE('',*,*,#7874,.T.) ;
#10762 = ORIENTED_EDGE('',*,*,#7875,.T.) ;
#10763 = ORIENTED_EDGE('',*,*,#7876,.T.) ;
#10764 = ORIENTED_EDGE('',*,*,#7877,.T.) ;
#10765 = ORIENTED_EDGE('',*,*,#7854,.T.) ;
#10766 = ORIENTED_EDGE('',*,*,#7868,.T.) ;
#10767 = ORIENTED_EDGE('',*,*,#7864,.T.) ;
#10768 = ORIENTED_EDGE('',*,*,#7860,.T.) ;
#10769 = ORIENTED_EDGE('',*,*,#7874,.F.) ;
#10770 = ORIENTED_EDGE('',*,*,#7878,.T.) ;
#10771 = ORIENTED_EDGE('',*,*,#7870,.T.) ;
#10772 = ORIENTED_EDGE('',*,*,#7879,.F.) ;
#10773 = ORIENTED_EDGE('',*,*,#7875,.F.) ;
#10774 = ORIENTED_EDGE('',*,*,#7879,.T.) ;
#10775 = ORIENTED_EDGE('',*,*,#7873,.T.) ;
#10776 = ORIENTED_EDGE('',*,*,#7880,.F.) ;
#10777 = ORIENTED_EDGE('',*,*,#7876,.F.) ;
#10778 = ORIENTED_EDGE('',*,*,#7880,.T.) ;
#10779 = ORIENTED_EDGE('',*,*,#7872,.T.) ;
#10780 = ORIENTED_EDGE('',*,*,#7881,.F.) ;
#10781 = ORIENTED_EDGE('',*,*,#7877,.F.) ;
#10782 = ORIENTED_EDGE('',*,*,#7881,.T.) ;
#10783 = ORIENTED_EDGE('',*,*,#7871,.T.) ;
#10784 = ORIENTED_EDGE('',*,*,#7878,.F.) ;
#10785 = ORIENTED_EDGE('',*,*,#7882,.F.) ;
#10786 = ORIENTED_EDGE('',*,*,#7883,.T.) ;
#10787 = ORIENTED_EDGE('',*,*,#7884,.F.) ;
#10788 = ORIENTED_EDGE('',*,*,#7883,.F.) ;
#10789 = ORIENTED_EDGE('',*,*,#7882,.T.) ;
#10790 = ORIENTED_EDGE('',*,*,#7885,.F.) ;
#10791 = ORIENTED_EDGE('',*,*,#7886,.F.) ;
#10792 = ORIENTED_EDGE('',*,*,#7887,.T.) ;
#10793 = ORIENTED_EDGE('',*,*,#7888,.T.) ;
#10794 = ORIENTED_EDGE('',*,*,#7889,.F.) ;
#10795 = ORIENTED_EDGE('',*,*,#7888,.F.) ;
#10796 = ORIENTED_EDGE('',*,*,#7890,.T.) ;
#10797 = ORIENTED_EDGE('',*,*,#7891,.T.) ;
#10798 = ORIENTED_EDGE('',*,*,#7892,.F.) ;
#10799 = ORIENTED_EDGE('',*,*,#7893,.F.) ;
#10800 = ORIENTED_EDGE('',*,*,#7890,.F.) ;
#10801 = ORIENTED_EDGE('',*,*,#7887,.F.) ;
#10802 = ORIENTED_EDGE('',*,*,#7894,.F.) ;
#10803 = ORIENTED_EDGE('',*,*,#7891,.F.) ;
#10804 = ORIENTED_EDGE('',*,*,#7893,.T.) ;
#10805 = ORIENTED_EDGE('',*,*,#7895,.T.) ;
#10806 = ORIENTED_EDGE('',*,*,#7896,.F.) ;
#10807 = ORIENTED_EDGE('',*,*,#7895,.F.) ;
#10808 = ORIENTED_EDGE('',*,*,#7892,.T.) ;
#10809 = ORIENTED_EDGE('',*,*,#7886,.T.) ;
#10810 = ORIENTED_EDGE('',*,*,#7897,.T.) ;
#10811 = ORIENTED_EDGE('',*,*,#7898,.T.) ;
#10812 = ORIENTED_EDGE('',*,*,#7899,.T.) ;
#10813 = ORIENTED_EDGE('',*,*,#7900,.T.) ;
#10814 = ORIENTED_EDGE('',*,*,#7894,.T.) ;
#10815 = ORIENTED_EDGE('',*,*,#7896,.T.) ;
#10816 = ORIENTED_EDGE('',*,*,#7885,.T.) ;
#10817 = ORIENTED_EDGE('',*,*,#7889,.T.) ;
#10818 = ORIENTED_EDGE('',*,*,#7901,.T.) ;
#10819 = ORIENTED_EDGE('',*,*,#7898,.F.) ;
#10820 = ORIENTED_EDGE('',*,*,#7902,.F.) ;
#10821 = ORIENTED_EDGE('',*,*,#7903,.F.) ;
#10822 = ORIENTED_EDGE('',*,*,#7904,.T.) ;
#10823 = ORIENTED_EDGE('',*,*,#7899,.F.) ;
#10824 = ORIENTED_EDGE('',*,*,#7901,.F.) ;
#10825 = ORIENTED_EDGE('',*,*,#7905,.F.) ;
#10826 = ORIENTED_EDGE('',*,*,#7906,.T.) ;
#10827 = ORIENTED_EDGE('',*,*,#7900,.F.) ;
#10828 = ORIENTED_EDGE('',*,*,#7904,.F.) ;
#10829 = ORIENTED_EDGE('',*,*,#7907,.F.) ;
#10830 = ORIENTED_EDGE('',*,*,#7902,.T.) ;
#10831 = ORIENTED_EDGE('',*,*,#7897,.F.) ;
#10832 = ORIENTED_EDGE('',*,*,#7906,.F.) ;
#10833 = ORIENTED_EDGE('',*,*,#7908,.F.) ;
#10834 = ORIENTED_EDGE('',*,*,#7909,.T.) ;
#10835 = ORIENTED_EDGE('',*,*,#7910,.T.) ;
#10836 = ORIENTED_EDGE('',*,*,#7911,.T.) ;
#10837 = ORIENTED_EDGE('',*,*,#7912,.T.) ;
#10838 = ORIENTED_EDGE('',*,*,#7884,.T.) ;
#10839 = ORIENTED_EDGE('',*,*,#7913,.T.) ;
#10840 = ORIENTED_EDGE('',*,*,#7914,.T.) ;
#10841 = ORIENTED_EDGE('',*,*,#7915,.T.) ;
#10842 = ORIENTED_EDGE('',*,*,#7916,.T.) ;
#10843 = ORIENTED_EDGE('',*,*,#7903,.T.) ;
#10844 = ORIENTED_EDGE('',*,*,#7908,.T.) ;
#10845 = ORIENTED_EDGE('',*,*,#7907,.T.) ;
#10846 = ORIENTED_EDGE('',*,*,#7905,.T.) ;
#10847 = ORIENTED_EDGE('',*,*,#7917,.T.) ;
#10848 = ORIENTED_EDGE('',*,*,#7914,.F.) ;
#10849 = ORIENTED_EDGE('',*,*,#7918,.F.) ;
#10850 = ORIENTED_EDGE('',*,*,#7912,.F.) ;
#10851 = ORIENTED_EDGE('',*,*,#7919,.T.) ;
#10852 = ORIENTED_EDGE('',*,*,#7915,.F.) ;
#10853 = ORIENTED_EDGE('',*,*,#7917,.F.) ;
#10854 = ORIENTED_EDGE('',*,*,#7911,.F.) ;
#10855 = ORIENTED_EDGE('',*,*,#7920,.T.) ;
#10856 = ORIENTED_EDGE('',*,*,#7916,.F.) ;
#10857 = ORIENTED_EDGE('',*,*,#7919,.F.) ;
#10858 = ORIENTED_EDGE('',*,*,#7910,.F.) ;
#10859 = ORIENTED_EDGE('',*,*,#7918,.T.) ;
#10860 = ORIENTED_EDGE('',*,*,#7913,.F.) ;
#10861 = ORIENTED_EDGE('',*,*,#7920,.F.) ;
#10862 = ORIENTED_EDGE('',*,*,#7909,.F.) ;
#10863 = ORIENTED_EDGE('',*,*,#7921,.F.) ;
#10864 = ORIENTED_EDGE('',*,*,#7922,.T.) ;
#10865 = ORIENTED_EDGE('',*,*,#7923,.T.) ;
#10866 = ORIENTED_EDGE('',*,*,#7924,.T.) ;
#10867 = ORIENTED_EDGE('',*,*,#7925,.F.) ;
#10868 = ORIENTED_EDGE('',*,*,#7926,.T.) ;
#10869 = ORIENTED_EDGE('',*,*,#7927,.F.) ;
#10870 = ORIENTED_EDGE('',*,*,#7928,.F.) ;
#10871 = ORIENTED_EDGE('',*,*,#7929,.F.) ;
#10872 = ORIENTED_EDGE('',*,*,#7930,.F.) ;
#10873 = ORIENTED_EDGE('',*,*,#7931,.F.) ;
#10874 = ORIENTED_EDGE('',*,*,#7932,.F.) ;
#10875 = ORIENTED_EDGE('',*,*,#7933,.F.) ;
#10876 = ORIENTED_EDGE('',*,*,#7934,.F.) ;
#10877 = ORIENTED_EDGE('',*,*,#7935,.F.) ;
#10878 = ORIENTED_EDGE('',*,*,#7936,.T.) ;
#10879 = ORIENTED_EDGE('',*,*,#7937,.T.) ;
#10880 = ORIENTED_EDGE('',*,*,#7930,.T.) ;
#10881 = ORIENTED_EDGE('',*,*,#7938,.F.) ;
#10882 = ORIENTED_EDGE('',*,*,#7932,.T.) ;
#10883 = ORIENTED_EDGE('',*,*,#7939,.F.) ;
#10884 = ORIENTED_EDGE('',*,*,#7940,.T.) ;
#10885 = ORIENTED_EDGE('',*,*,#7941,.F.) ;
#10886 = ORIENTED_EDGE('',*,*,#7942,.F.) ;
#10887 = ORIENTED_EDGE('',*,*,#7943,.F.) ;
#10888 = ORIENTED_EDGE('',*,*,#7944,.T.) ;
#10889 = ORIENTED_EDGE('',*,*,#7925,.T.) ;
#10890 = ORIENTED_EDGE('',*,*,#7945,.T.) ;
#10891 = ORIENTED_EDGE('',*,*,#7946,.F.) ;
#10892 = ORIENTED_EDGE('',*,*,#7947,.F.) ;
#10893 = ORIENTED_EDGE('',*,*,#7948,.F.) ;
#10894 = ORIENTED_EDGE('',*,*,#7940,.F.) ;
#10895 = ORIENTED_EDGE('',*,*,#7949,.F.) ;
#10896 = ORIENTED_EDGE('',*,*,#7950,.F.) ;
#10897 = ORIENTED_EDGE('',*,*,#7926,.F.) ;
#10898 = ORIENTED_EDGE('',*,*,#7944,.F.) ;
#10899 = ORIENTED_EDGE('',*,*,#7951,.F.) ;
#10900 = ORIENTED_EDGE('',*,*,#7952,.F.) ;
#10901 = ORIENTED_EDGE('',*,*,#7936,.F.) ;
#10902 = ORIENTED_EDGE('',*,*,#7953,.F.) ;
#10903 = ORIENTED_EDGE('',*,*,#7954,.F.) ;
#10904 = ORIENTED_EDGE('',*,*,#7922,.F.) ;
#10905 = ORIENTED_EDGE('',*,*,#7955,.F.) ;
#10906 = ORIENTED_EDGE('',*,*,#7945,.F.) ;
#10907 = ORIENTED_EDGE('',*,*,#7924,.F.) ;
#10908 = ORIENTED_EDGE('',*,*,#7956,.F.) ;
#10909 = ORIENTED_EDGE('',*,*,#7957,.F.) ;
#10910 = ORIENTED_EDGE('',*,*,#7958,.F.) ;
#10911 = ORIENTED_EDGE('',*,*,#7959,.F.) ;
#10912 = ORIENTED_EDGE('',*,*,#7956,.T.) ;
#10913 = ORIENTED_EDGE('',*,*,#7923,.F.) ;
#10914 = ORIENTED_EDGE('',*,*,#7954,.T.) ;
#10915 = ORIENTED_EDGE('',*,*,#7960,.F.) ;
#10916 = ORIENTED_EDGE('',*,*,#7961,.F.) ;
#10917 = ORIENTED_EDGE('',*,*,#7962,.F.) ;
#10918 = ORIENTED_EDGE('',*,*,#7949,.T.) ;
#10919 = ORIENTED_EDGE('',*,*,#7939,.T.) ;
#10920 = ORIENTED_EDGE('',*,*,#7931,.T.) ;
#10921 = ORIENTED_EDGE('',*,*,#7937,.F.) ;
#10922 = ORIENTED_EDGE('',*,*,#7952,.T.) ;
#10923 = ORIENTED_EDGE('',*,*,#7947,.T.) ;
#10924 = ORIENTED_EDGE('',*,*,#7963,.T.) ;
#10925 = ORIENTED_EDGE('',*,*,#7964,.F.) ;
#10926 = ORIENTED_EDGE('',*,*,#7958,.T.) ;
#10927 = ORIENTED_EDGE('',*,*,#7965,.F.) ;
#10928 = ORIENTED_EDGE('',*,*,#7966,.T.) ;
#10929 = ORIENTED_EDGE('',*,*,#7928,.T.) ;
#10930 = ORIENTED_EDGE('',*,*,#7967,.F.) ;
#10931 = ORIENTED_EDGE('',*,*,#7968,.F.) ;
#10932 = ORIENTED_EDGE('',*,*,#7942,.T.) ;
#10933 = ORIENTED_EDGE('',*,*,#7969,.F.) ;
#10934 = ORIENTED_EDGE('',*,*,#7970,.T.) ;
#10935 = ORIENTED_EDGE('',*,*,#7961,.T.) ;
#10936 = ORIENTED_EDGE('',*,*,#7971,.F.) ;
#10937 = ORIENTED_EDGE('',*,*,#7972,.F.) ;
#10938 = ORIENTED_EDGE('',*,*,#7973,.T.) ;
#10939 = ORIENTED_EDGE('',*,*,#7974,.F.) ;
#10940 = ORIENTED_EDGE('',*,*,#7975,.F.) ;
#10941 = ORIENTED_EDGE('',*,*,#7973,.F.) ;
#10942 = ORIENTED_EDGE('',*,*,#7976,.F.) ;
#10943 = ORIENTED_EDGE('',*,*,#7977,.T.) ;
#10944 = ORIENTED_EDGE('',*,*,#7978,.F.) ;
#10945 = ORIENTED_EDGE('',*,*,#7977,.F.) ;
#10946 = ORIENTED_EDGE('',*,*,#7979,.F.) ;
#10947 = ORIENTED_EDGE('',*,*,#7980,.T.) ;
#10948 = ORIENTED_EDGE('',*,*,#7981,.F.) ;
#10949 = ORIENTED_EDGE('',*,*,#7980,.F.) ;
#10950 = ORIENTED_EDGE('',*,*,#7982,.T.) ;
#10951 = ORIENTED_EDGE('',*,*,#7983,.T.) ;
#10952 = ORIENTED_EDGE('',*,*,#7984,.T.) ;
#10953 = ORIENTED_EDGE('',*,*,#7983,.F.) ;
#10954 = ORIENTED_EDGE('',*,*,#7959,.T.) ;
#10955 = ORIENTED_EDGE('',*,*,#7966,.F.) ;
#10956 = ORIENTED_EDGE('',*,*,#7985,.F.) ;
#10957 = ORIENTED_EDGE('',*,*,#7986,.F.) ;
#10958 = ORIENTED_EDGE('',*,*,#7933,.T.) ;
#10959 = ORIENTED_EDGE('',*,*,#7929,.T.) ;
#10960 = ORIENTED_EDGE('',*,*,#7938,.T.) ;
#10961 = ORIENTED_EDGE('',*,*,#7970,.F.) ;
#10962 = ORIENTED_EDGE('',*,*,#7987,.F.) ;
#10963 = ORIENTED_EDGE('',*,*,#7963,.F.) ;
#10964 = ORIENTED_EDGE('',*,*,#7946,.T.) ;
#10965 = ORIENTED_EDGE('',*,*,#7955,.T.) ;
#10966 = ORIENTED_EDGE('',*,*,#7974,.T.) ;
#10967 = ORIENTED_EDGE('',*,*,#7975,.T.) ;
#10968 = ORIENTED_EDGE('',*,*,#7982,.F.) ;
#10969 = ORIENTED_EDGE('',*,*,#7981,.T.) ;
#10970 = ORIENTED_EDGE('',*,*,#7984,.F.) ;
#10971 = ORIENTED_EDGE('',*,*,#7976,.T.) ;
#10972 = ORIENTED_EDGE('',*,*,#7934,.T.) ;
#10973 = ORIENTED_EDGE('',*,*,#7986,.T.) ;
#10974 = ORIENTED_EDGE('',*,*,#7988,.F.) ;
#10975 = ORIENTED_EDGE('',*,*,#7921,.T.) ;
#10976 = ORIENTED_EDGE('',*,*,#7968,.T.) ;
#10977 = ORIENTED_EDGE('',*,*,#7989,.T.) ;
#10978 = ORIENTED_EDGE('',*,*,#7990,.F.) ;
#10979 = ORIENTED_EDGE('',*,*,#7989,.F.) ;
#10980 = ORIENTED_EDGE('',*,*,#7967,.T.) ;
#10981 = ORIENTED_EDGE('',*,*,#7927,.T.) ;
#10982 = ORIENTED_EDGE('',*,*,#7950,.T.) ;
#10983 = ORIENTED_EDGE('',*,*,#7943,.T.) ;
#10984 = ORIENTED_EDGE('',*,*,#7964,.T.) ;
#10985 = ORIENTED_EDGE('',*,*,#7987,.T.) ;
#10986 = ORIENTED_EDGE('',*,*,#7969,.T.) ;
#10987 = ORIENTED_EDGE('',*,*,#7941,.T.) ;
#10988 = ORIENTED_EDGE('',*,*,#7948,.T.) ;
#10989 = ORIENTED_EDGE('',*,*,#7962,.T.) ;
#10990 = ORIENTED_EDGE('',*,*,#7971,.T.) ;
#10991 = ORIENTED_EDGE('',*,*,#7960,.T.) ;
#10992 = ORIENTED_EDGE('',*,*,#7951,.T.) ;
#10993 = ORIENTED_EDGE('',*,*,#7935,.T.) ;
#10994 = ORIENTED_EDGE('',*,*,#7988,.T.) ;
#10995 = ORIENTED_EDGE('',*,*,#7985,.T.) ;
#10996 = ORIENTED_EDGE('',*,*,#7965,.T.) ;
#10997 = ORIENTED_EDGE('',*,*,#7957,.T.) ;
#10998 = ORIENTED_EDGE('',*,*,#7953,.T.) ;
#10999 = ORIENTED_EDGE('',*,*,#7991,.T.) ;
#11000 = ORIENTED_EDGE('',*,*,#7992,.T.) ;
#11001 = ORIENTED_EDGE('',*,*,#7993,.T.) ;
#11002 = ORIENTED_EDGE('',*,*,#7994,.T.) ;
#11003 = ORIENTED_EDGE('',*,*,#7990,.T.) ;
#11004 = ORIENTED_EDGE('',*,*,#7995,.T.) ;
#11005 = ORIENTED_EDGE('',*,*,#7996,.T.) ;
#11006 = ORIENTED_EDGE('',*,*,#7997,.T.) ;
#11007 = ORIENTED_EDGE('',*,*,#7998,.T.) ;
#11008 = ORIENTED_EDGE('',*,*,#7972,.T.) ;
#11009 = ORIENTED_EDGE('',*,*,#7999,.T.) ;
#11010 = ORIENTED_EDGE('',*,*,#7996,.F.) ;
#11011 = ORIENTED_EDGE('',*,*,#8000,.F.) ;
#11012 = ORIENTED_EDGE('',*,*,#7994,.F.) ;
#11013 = ORIENTED_EDGE('',*,*,#7979,.T.) ;
#11014 = ORIENTED_EDGE('',*,*,#8001,.T.) ;
#11015 = ORIENTED_EDGE('',*,*,#7997,.F.) ;
#11016 = ORIENTED_EDGE('',*,*,#7999,.F.) ;
#11017 = ORIENTED_EDGE('',*,*,#7993,.F.) ;
#11018 = ORIENTED_EDGE('',*,*,#8002,.T.) ;
#11019 = ORIENTED_EDGE('',*,*,#7998,.F.) ;
#11020 = ORIENTED_EDGE('',*,*,#8001,.F.) ;
#11021 = ORIENTED_EDGE('',*,*,#7992,.F.) ;
#11022 = ORIENTED_EDGE('',*,*,#7978,.T.) ;
#11023 = ORIENTED_EDGE('',*,*,#8000,.T.) ;
#11024 = ORIENTED_EDGE('',*,*,#7995,.F.) ;
#11025 = ORIENTED_EDGE('',*,*,#8002,.F.) ;
#11026 = ORIENTED_EDGE('',*,*,#7991,.F.) ;
#11027 = ORIENTED_EDGE('',*,*,#8003,.F.) ;
#11028 = ORIENTED_EDGE('',*,*,#8004,.T.) ;
#11029 = ORIENTED_EDGE('',*,*,#8005,.F.) ;
#11030 = ORIENTED_EDGE('',*,*,#8004,.F.) ;
#11031 = ORIENTED_EDGE('',*,*,#8006,.F.) ;
#11032 = ORIENTED_EDGE('',*,*,#8007,.F.) ;
#11033 = ORIENTED_EDGE('',*,*,#8008,.F.) ;
#11034 = ORIENTED_EDGE('',*,*,#8009,.F.) ;
#11035 = ORIENTED_EDGE('',*,*,#8008,.T.) ;
#11036 = ORIENTED_EDGE('',*,*,#8010,.T.) ;
#11037 = ORIENTED_EDGE('',*,*,#8011,.T.) ;
#11038 = ORIENTED_EDGE('',*,*,#8012,.T.) ;
#11039 = ORIENTED_EDGE('',*,*,#8013,.T.) ;
#11040 = ORIENTED_EDGE('',*,*,#8014,.T.) ;
#11041 = ORIENTED_EDGE('',*,*,#8015,.T.) ;
#11042 = ORIENTED_EDGE('',*,*,#8016,.T.) ;
#11043 = ORIENTED_EDGE('',*,*,#8017,.T.) ;
#11044 = ORIENTED_EDGE('',*,*,#8018,.T.) ;
#11045 = ORIENTED_EDGE('',*,*,#8019,.T.) ;
#11046 = ORIENTED_EDGE('',*,*,#8020,.T.) ;
#11047 = ORIENTED_EDGE('',*,*,#8021,.T.) ;
#11048 = ORIENTED_EDGE('',*,*,#8022,.T.) ;
#11049 = ORIENTED_EDGE('',*,*,#8023,.T.) ;
#11050 = ORIENTED_EDGE('',*,*,#8024,.T.) ;
#11051 = ORIENTED_EDGE('',*,*,#8005,.T.) ;
#11052 = ORIENTED_EDGE('',*,*,#8007,.T.) ;
#11053 = ORIENTED_EDGE('',*,*,#8025,.F.) ;
#11054 = ORIENTED_EDGE('',*,*,#8026,.T.) ;
#11055 = ORIENTED_EDGE('',*,*,#8010,.F.) ;
#11056 = ORIENTED_EDGE('',*,*,#8027,.F.) ;
#11057 = ORIENTED_EDGE('',*,*,#8028,.F.) ;
#11058 = ORIENTED_EDGE('',*,*,#8011,.F.) ;
#11059 = ORIENTED_EDGE('',*,*,#8026,.F.) ;
#11060 = ORIENTED_EDGE('',*,*,#8028,.T.) ;
#11061 = ORIENTED_EDGE('',*,*,#8029,.F.) ;
#11062 = ORIENTED_EDGE('',*,*,#8030,.T.) ;
#11063 = ORIENTED_EDGE('',*,*,#8012,.F.) ;
#11064 = ORIENTED_EDGE('',*,*,#8031,.F.) ;
#11065 = ORIENTED_EDGE('',*,*,#8032,.F.) ;
#11066 = ORIENTED_EDGE('',*,*,#8013,.F.) ;
#11067 = ORIENTED_EDGE('',*,*,#8030,.F.) ;
#11068 = ORIENTED_EDGE('',*,*,#8032,.T.) ;
#11069 = ORIENTED_EDGE('',*,*,#8033,.F.) ;
#11070 = ORIENTED_EDGE('',*,*,#8034,.T.) ;
#11071 = ORIENTED_EDGE('',*,*,#8014,.F.) ;
#11072 = ORIENTED_EDGE('',*,*,#8035,.F.) ;
#11073 = ORIENTED_EDGE('',*,*,#8036,.F.) ;
#11074 = ORIENTED_EDGE('',*,*,#8015,.F.) ;
#11075 = ORIENTED_EDGE('',*,*,#8034,.F.) ;
#11076 = ORIENTED_EDGE('',*,*,#8036,.T.) ;
#11077 = ORIENTED_EDGE('',*,*,#8037,.F.) ;
#11078 = ORIENTED_EDGE('',*,*,#8038,.T.) ;
#11079 = ORIENTED_EDGE('',*,*,#8016,.F.) ;
#11080 = ORIENTED_EDGE('',*,*,#8039,.F.) ;
#11081 = ORIENTED_EDGE('',*,*,#8040,.F.) ;
#11082 = ORIENTED_EDGE('',*,*,#8017,.F.) ;
#11083 = ORIENTED_EDGE('',*,*,#8038,.F.) ;
#11084 = ORIENTED_EDGE('',*,*,#8040,.T.) ;
#11085 = ORIENTED_EDGE('',*,*,#8041,.F.) ;
#11086 = ORIENTED_EDGE('',*,*,#8042,.T.) ;
#11087 = ORIENTED_EDGE('',*,*,#8018,.F.) ;
#11088 = ORIENTED_EDGE('',*,*,#8043,.F.) ;
#11089 = ORIENTED_EDGE('',*,*,#8044,.F.) ;
#11090 = ORIENTED_EDGE('',*,*,#8019,.F.) ;
#11091 = ORIENTED_EDGE('',*,*,#8042,.F.) ;
#11092 = ORIENTED_EDGE('',*,*,#8044,.T.) ;
#11093 = ORIENTED_EDGE('',*,*,#8045,.F.) ;
#11094 = ORIENTED_EDGE('',*,*,#8046,.T.) ;
#11095 = ORIENTED_EDGE('',*,*,#8020,.F.) ;
#11096 = ORIENTED_EDGE('',*,*,#8047,.F.) ;
#11097 = ORIENTED_EDGE('',*,*,#8048,.F.) ;
#11098 = ORIENTED_EDGE('',*,*,#8021,.F.) ;
#11099 = ORIENTED_EDGE('',*,*,#8046,.F.) ;
#11100 = ORIENTED_EDGE('',*,*,#8048,.T.) ;
#11101 = ORIENTED_EDGE('',*,*,#8049,.F.) ;
#11102 = ORIENTED_EDGE('',*,*,#8050,.T.) ;
#11103 = ORIENTED_EDGE('',*,*,#8022,.F.) ;
#11104 = ORIENTED_EDGE('',*,*,#8050,.F.) ;
#11105 = ORIENTED_EDGE('',*,*,#8051,.F.) ;
#11106 = ORIENTED_EDGE('',*,*,#8052,.F.) ;
#11107 = ORIENTED_EDGE('',*,*,#8023,.F.) ;
#11108 = ORIENTED_EDGE('',*,*,#8006,.T.) ;
#11109 = ORIENTED_EDGE('',*,*,#8053,.T.) ;
#11110 = ORIENTED_EDGE('',*,*,#8051,.T.) ;
#11111 = ORIENTED_EDGE('',*,*,#8049,.T.) ;
#11112 = ORIENTED_EDGE('',*,*,#8047,.T.) ;
#11113 = ORIENTED_EDGE('',*,*,#8045,.T.) ;
#11114 = ORIENTED_EDGE('',*,*,#8043,.T.) ;
#11115 = ORIENTED_EDGE('',*,*,#8041,.T.) ;
#11116 = ORIENTED_EDGE('',*,*,#8039,.T.) ;
#11117 = ORIENTED_EDGE('',*,*,#8037,.T.) ;
#11118 = ORIENTED_EDGE('',*,*,#8035,.T.) ;
#11119 = ORIENTED_EDGE('',*,*,#8033,.T.) ;
#11120 = ORIENTED_EDGE('',*,*,#8031,.T.) ;
#11121 = ORIENTED_EDGE('',*,*,#8029,.T.) ;
#11122 = ORIENTED_EDGE('',*,*,#8027,.T.) ;
#11123 = ORIENTED_EDGE('',*,*,#8025,.T.) ;
#11124 = ORIENTED_EDGE('',*,*,#8003,.T.) ;
#11125 = ORIENTED_EDGE('',*,*,#8009,.T.) ;
#11126 = ORIENTED_EDGE('',*,*,#8024,.F.) ;
#11127 = ORIENTED_EDGE('',*,*,#8052,.T.) ;
#11128 = ORIENTED_EDGE('',*,*,#8053,.F.) ;
#11129 = ORIENTED_EDGE('',*,*,#8054,.F.) ;
#11130 = ORIENTED_EDGE('',*,*,#8055,.T.) ;
#11131 = ORIENTED_EDGE('',*,*,#8056,.F.) ;
#11132 = ORIENTED_EDGE('',*,*,#8055,.F.) ;
#11133 = ORIENTED_EDGE('',*,*,#8056,.T.) ;
#11134 = ORIENTED_EDGE('',*,*,#8054,.T.) ;
#11135 = ORIENTED_EDGE('',*,*,#8057,.F.) ;
#11136 = ORIENTED_EDGE('',*,*,#8058,.T.) ;
#11137 = ORIENTED_EDGE('',*,*,#8059,.F.) ;
#11138 = ORIENTED_EDGE('',*,*,#8058,.F.) ;
#11139 = ORIENTED_EDGE('',*,*,#8060,.F.) ;
#11140 = ORIENTED_EDGE('',*,*,#8061,.T.) ;
#11141 = ORIENTED_EDGE('',*,*,#8062,.F.) ;
#11142 = ORIENTED_EDGE('',*,*,#8061,.F.) ;
#11143 = ORIENTED_EDGE('',*,*,#8062,.T.) ;
#11144 = ORIENTED_EDGE('',*,*,#8057,.T.) ;
#11145 = ORIENTED_EDGE('',*,*,#8060,.T.) ;
#11146 = ORIENTED_EDGE('',*,*,#8059,.T.) ;
#11147 = ORIENTED_EDGE('',*,*,#8063,.F.) ;
#11148 = ORIENTED_EDGE('',*,*,#8064,.T.) ;
#11149 = ORIENTED_EDGE('',*,*,#8065,.F.) ;
#11150 = ORIENTED_EDGE('',*,*,#8064,.F.) ;
#11151 = ORIENTED_EDGE('',*,*,#8066,.F.) ;
#11152 = ORIENTED_EDGE('',*,*,#8067,.T.) ;
#11153 = ORIENTED_EDGE('',*,*,#8068,.F.) ;
#11154 = ORIENTED_EDGE('',*,*,#8067,.F.) ;
#11155 = ORIENTED_EDGE('',*,*,#8068,.T.) ;
#11156 = ORIENTED_EDGE('',*,*,#8063,.T.) ;
#11157 = ORIENTED_EDGE('',*,*,#8069,.F.) ;
#11158 = ORIENTED_EDGE('',*,*,#8070,.F.) ;
#11159 = ORIENTED_EDGE('',*,*,#8071,.F.) ;
#11160 = ORIENTED_EDGE('',*,*,#8072,.F.) ;
#11161 = ORIENTED_EDGE('',*,*,#8073,.F.) ;
#11162 = ORIENTED_EDGE('',*,*,#8074,.T.) ;
#11163 = ORIENTED_EDGE('',*,*,#8075,.T.) ;
#11164 = ORIENTED_EDGE('',*,*,#8070,.T.) ;
#11165 = ORIENTED_EDGE('',*,*,#8076,.F.) ;
#11166 = ORIENTED_EDGE('',*,*,#8072,.T.) ;
#11167 = ORIENTED_EDGE('',*,*,#8077,.T.) ;
#11168 = ORIENTED_EDGE('',*,*,#8078,.T.) ;
#11169 = ORIENTED_EDGE('',*,*,#8079,.F.) ;
#11170 = ORIENTED_EDGE('',*,*,#8078,.F.) ;
#11171 = ORIENTED_EDGE('',*,*,#8080,.T.) ;
#11172 = ORIENTED_EDGE('',*,*,#8074,.F.) ;
#11173 = ORIENTED_EDGE('',*,*,#8071,.T.) ;
#11174 = ORIENTED_EDGE('',*,*,#8075,.F.) ;
#11175 = ORIENTED_EDGE('',*,*,#8080,.F.) ;
#11176 = ORIENTED_EDGE('',*,*,#8077,.F.) ;
#11177 = ORIENTED_EDGE('',*,*,#8081,.F.) ;
#11178 = ORIENTED_EDGE('',*,*,#8082,.F.) ;
#11179 = ORIENTED_EDGE('',*,*,#8083,.F.) ;
#11180 = ORIENTED_EDGE('',*,*,#8084,.F.) ;
#11181 = ORIENTED_EDGE('',*,*,#8085,.F.) ;
#11182 = ORIENTED_EDGE('',*,*,#8086,.T.) ;
#11183 = ORIENTED_EDGE('',*,*,#8087,.T.) ;
#11184 = ORIENTED_EDGE('',*,*,#8082,.T.) ;
#11185 = ORIENTED_EDGE('',*,*,#8088,.F.) ;
#11186 = ORIENTED_EDGE('',*,*,#8084,.T.) ;
#11187 = ORIENTED_EDGE('',*,*,#8089,.T.) ;
#11188 = ORIENTED_EDGE('',*,*,#8090,.T.) ;
#11189 = ORIENTED_EDGE('',*,*,#8091,.F.) ;
#11190 = ORIENTED_EDGE('',*,*,#8090,.F.) ;
#11191 = ORIENTED_EDGE('',*,*,#8092,.T.) ;
#11192 = ORIENTED_EDGE('',*,*,#8086,.F.) ;
#11193 = ORIENTED_EDGE('',*,*,#8083,.T.) ;
#11194 = ORIENTED_EDGE('',*,*,#8087,.F.) ;
#11195 = ORIENTED_EDGE('',*,*,#8092,.F.) ;
#11196 = ORIENTED_EDGE('',*,*,#8089,.F.) ;
#11197 = ORIENTED_EDGE('',*,*,#8093,.F.) ;
#11198 = ORIENTED_EDGE('',*,*,#8094,.F.) ;
#11199 = ORIENTED_EDGE('',*,*,#8095,.F.) ;
#11200 = ORIENTED_EDGE('',*,*,#8096,.F.) ;
#11201 = ORIENTED_EDGE('',*,*,#8097,.F.) ;
#11202 = ORIENTED_EDGE('',*,*,#8098,.T.) ;
#11203 = ORIENTED_EDGE('',*,*,#8099,.T.) ;
#11204 = ORIENTED_EDGE('',*,*,#8094,.T.) ;
#11205 = ORIENTED_EDGE('',*,*,#8100,.F.) ;
#11206 = ORIENTED_EDGE('',*,*,#8096,.T.) ;
#11207 = ORIENTED_EDGE('',*,*,#8101,.T.) ;
#11208 = ORIENTED_EDGE('',*,*,#8102,.T.) ;
#11209 = ORIENTED_EDGE('',*,*,#8103,.F.) ;
#11210 = ORIENTED_EDGE('',*,*,#8102,.F.) ;
#11211 = ORIENTED_EDGE('',*,*,#8104,.T.) ;
#11212 = ORIENTED_EDGE('',*,*,#8098,.F.) ;
#11213 = ORIENTED_EDGE('',*,*,#8095,.T.) ;
#11214 = ORIENTED_EDGE('',*,*,#8099,.F.) ;
#11215 = ORIENTED_EDGE('',*,*,#8104,.F.) ;
#11216 = ORIENTED_EDGE('',*,*,#8101,.F.) ;
#11217 = ORIENTED_EDGE('',*,*,#8105,.F.) ;
#11218 = ORIENTED_EDGE('',*,*,#8106,.F.) ;
#11219 = ORIENTED_EDGE('',*,*,#8107,.F.) ;
#11220 = ORIENTED_EDGE('',*,*,#8108,.F.) ;
#11221 = ORIENTED_EDGE('',*,*,#8109,.F.) ;
#11222 = ORIENTED_EDGE('',*,*,#8110,.T.) ;
#11223 = ORIENTED_EDGE('',*,*,#8111,.T.) ;
#11224 = ORIENTED_EDGE('',*,*,#8106,.T.) ;
#11225 = ORIENTED_EDGE('',*,*,#8112,.F.) ;
#11226 = ORIENTED_EDGE('',*,*,#8108,.T.) ;
#11227 = ORIENTED_EDGE('',*,*,#8113,.T.) ;
#11228 = ORIENTED_EDGE('',*,*,#8114,.T.) ;
#11229 = ORIENTED_EDGE('',*,*,#8115,.F.) ;
#11230 = ORIENTED_EDGE('',*,*,#8114,.F.) ;
#11231 = ORIENTED_EDGE('',*,*,#8116,.T.) ;
#11232 = ORIENTED_EDGE('',*,*,#8110,.F.) ;
#11233 = ORIENTED_EDGE('',*,*,#8107,.T.) ;
#11234 = ORIENTED_EDGE('',*,*,#8111,.F.) ;
#11235 = ORIENTED_EDGE('',*,*,#8116,.F.) ;
#11236 = ORIENTED_EDGE('',*,*,#8113,.F.) ;
#11237 = ORIENTED_EDGE('',*,*,#8117,.F.) ;
#11238 = ORIENTED_EDGE('',*,*,#8118,.F.) ;
#11239 = ORIENTED_EDGE('',*,*,#8119,.F.) ;
#11240 = ORIENTED_EDGE('',*,*,#8120,.F.) ;
#11241 = ORIENTED_EDGE('',*,*,#8121,.F.) ;
#11242 = ORIENTED_EDGE('',*,*,#8122,.F.) ;
#11243 = ORIENTED_EDGE('',*,*,#8123,.T.) ;
#11244 = ORIENTED_EDGE('',*,*,#8124,.T.) ;
#11245 = ORIENTED_EDGE('',*,*,#8118,.T.) ;
#11246 = ORIENTED_EDGE('',*,*,#8125,.F.) ;
#11247 = ORIENTED_EDGE('',*,*,#8120,.T.) ;
#11248 = ORIENTED_EDGE('',*,*,#8126,.T.) ;
#11249 = ORIENTED_EDGE('',*,*,#8127,.T.) ;
#11250 = ORIENTED_EDGE('',*,*,#8128,.F.) ;
#11251 = ORIENTED_EDGE('',*,*,#8127,.F.) ;
#11252 = ORIENTED_EDGE('',*,*,#8129,.T.) ;
#11253 = ORIENTED_EDGE('',*,*,#8123,.F.) ;
#11254 = ORIENTED_EDGE('',*,*,#8130,.F.) ;
#11255 = ORIENTED_EDGE('',*,*,#8119,.T.) ;
#11256 = ORIENTED_EDGE('',*,*,#8124,.F.) ;
#11257 = ORIENTED_EDGE('',*,*,#8129,.F.) ;
#11258 = ORIENTED_EDGE('',*,*,#8126,.F.) ;
#11259 = ORIENTED_EDGE('',*,*,#8131,.F.) ;
#11260 = ORIENTED_EDGE('',*,*,#8132,.F.) ;
#11261 = ORIENTED_EDGE('',*,*,#8133,.F.) ;
#11262 = ORIENTED_EDGE('',*,*,#8134,.F.) ;
#11263 = ORIENTED_EDGE('',*,*,#8135,.F.) ;
#11264 = ORIENTED_EDGE('',*,*,#8136,.T.) ;
#11265 = ORIENTED_EDGE('',*,*,#8137,.T.) ;
#11266 = ORIENTED_EDGE('',*,*,#8132,.T.) ;
#11267 = ORIENTED_EDGE('',*,*,#8138,.F.) ;
#11268 = ORIENTED_EDGE('',*,*,#8134,.T.) ;
#11269 = ORIENTED_EDGE('',*,*,#8139,.T.) ;
#11270 = ORIENTED_EDGE('',*,*,#8140,.T.) ;
#11271 = ORIENTED_EDGE('',*,*,#8141,.F.) ;
#11272 = ORIENTED_EDGE('',*,*,#8140,.F.) ;
#11273 = ORIENTED_EDGE('',*,*,#8142,.T.) ;
#11274 = ORIENTED_EDGE('',*,*,#8136,.F.) ;
#11275 = ORIENTED_EDGE('',*,*,#8133,.T.) ;
#11276 = ORIENTED_EDGE('',*,*,#8137,.F.) ;
#11277 = ORIENTED_EDGE('',*,*,#8142,.F.) ;
#11278 = ORIENTED_EDGE('',*,*,#8139,.F.) ;
#11279 = ORIENTED_EDGE('',*,*,#8143,.F.) ;
#11280 = ORIENTED_EDGE('',*,*,#8144,.F.) ;
#11281 = ORIENTED_EDGE('',*,*,#8145,.F.) ;
#11282 = ORIENTED_EDGE('',*,*,#8146,.F.) ;
#11283 = ORIENTED_EDGE('',*,*,#8147,.F.) ;
#11284 = ORIENTED_EDGE('',*,*,#8148,.T.) ;
#11285 = ORIENTED_EDGE('',*,*,#8149,.T.) ;
#11286 = ORIENTED_EDGE('',*,*,#8144,.T.) ;
#11287 = ORIENTED_EDGE('',*,*,#8150,.F.) ;
#11288 = ORIENTED_EDGE('',*,*,#8146,.T.) ;
#11289 = ORIENTED_EDGE('',*,*,#8151,.T.) ;
#11290 = ORIENTED_EDGE('',*,*,#8152,.T.) ;
#11291 = ORIENTED_EDGE('',*,*,#8153,.F.) ;
#11292 = ORIENTED_EDGE('',*,*,#8152,.F.) ;
#11293 = ORIENTED_EDGE('',*,*,#8154,.T.) ;
#11294 = ORIENTED_EDGE('',*,*,#8148,.F.) ;
#11295 = ORIENTED_EDGE('',*,*,#8145,.T.) ;
#11296 = ORIENTED_EDGE('',*,*,#8149,.F.) ;
#11297 = ORIENTED_EDGE('',*,*,#8154,.F.) ;
#11298 = ORIENTED_EDGE('',*,*,#8151,.F.) ;
#11299 = ORIENTED_EDGE('',*,*,#8155,.F.) ;
#11300 = ORIENTED_EDGE('',*,*,#8156,.F.) ;
#11301 = ORIENTED_EDGE('',*,*,#8157,.F.) ;
#11302 = ORIENTED_EDGE('',*,*,#8158,.F.) ;
#11303 = ORIENTED_EDGE('',*,*,#8159,.F.) ;
#11304 = ORIENTED_EDGE('',*,*,#8160,.T.) ;
#11305 = ORIENTED_EDGE('',*,*,#8161,.T.) ;
#11306 = ORIENTED_EDGE('',*,*,#8156,.T.) ;
#11307 = ORIENTED_EDGE('',*,*,#8162,.F.) ;
#11308 = ORIENTED_EDGE('',*,*,#8158,.T.) ;
#11309 = ORIENTED_EDGE('',*,*,#8163,.T.) ;
#11310 = ORIENTED_EDGE('',*,*,#8164,.T.) ;
#11311 = ORIENTED_EDGE('',*,*,#8165,.F.) ;
#11312 = ORIENTED_EDGE('',*,*,#8164,.F.) ;
#11313 = ORIENTED_EDGE('',*,*,#8166,.T.) ;
#11314 = ORIENTED_EDGE('',*,*,#8160,.F.) ;
#11315 = ORIENTED_EDGE('',*,*,#8157,.T.) ;
#11316 = ORIENTED_EDGE('',*,*,#8161,.F.) ;
#11317 = ORIENTED_EDGE('',*,*,#8166,.F.) ;
#11318 = ORIENTED_EDGE('',*,*,#8163,.F.) ;
#11319 = ORIENTED_EDGE('',*,*,#8167,.F.) ;
#11320 = ORIENTED_EDGE('',*,*,#8168,.F.) ;
#11321 = ORIENTED_EDGE('',*,*,#8169,.F.) ;
#11322 = ORIENTED_EDGE('',*,*,#8170,.F.) ;
#11323 = ORIENTED_EDGE('',*,*,#8171,.F.) ;
#11324 = ORIENTED_EDGE('',*,*,#8172,.T.) ;
#11325 = ORIENTED_EDGE('',*,*,#8173,.T.) ;
#11326 = ORIENTED_EDGE('',*,*,#8168,.T.) ;
#11327 = ORIENTED_EDGE('',*,*,#8174,.F.) ;
#11328 = ORIENTED_EDGE('',*,*,#8170,.T.) ;
#11329 = ORIENTED_EDGE('',*,*,#8175,.T.) ;
#11330 = ORIENTED_EDGE('',*,*,#8176,.T.) ;
#11331 = ORIENTED_EDGE('',*,*,#8177,.F.) ;
#11332 = ORIENTED_EDGE('',*,*,#8176,.F.) ;
#11333 = ORIENTED_EDGE('',*,*,#8178,.T.) ;
#11334 = ORIENTED_EDGE('',*,*,#8172,.F.) ;
#11335 = ORIENTED_EDGE('',*,*,#8169,.T.) ;
#11336 = ORIENTED_EDGE('',*,*,#8173,.F.) ;
#11337 = ORIENTED_EDGE('',*,*,#8178,.F.) ;
#11338 = ORIENTED_EDGE('',*,*,#8175,.F.) ;
#11339 = ORIENTED_EDGE('',*,*,#8179,.F.) ;
#11340 = ORIENTED_EDGE('',*,*,#8180,.F.) ;
#11341 = ORIENTED_EDGE('',*,*,#8181,.F.) ;
#11342 = ORIENTED_EDGE('',*,*,#8182,.F.) ;
#11343 = ORIENTED_EDGE('',*,*,#8183,.F.) ;
#11344 = ORIENTED_EDGE('',*,*,#8184,.T.) ;
#11345 = ORIENTED_EDGE('',*,*,#8185,.T.) ;
#11346 = ORIENTED_EDGE('',*,*,#8180,.T.) ;
#11347 = ORIENTED_EDGE('',*,*,#8186,.F.) ;
#11348 = ORIENTED_EDGE('',*,*,#8182,.T.) ;
#11349 = ORIENTED_EDGE('',*,*,#8187,.T.) ;
#11350 = ORIENTED_EDGE('',*,*,#8188,.T.) ;
#11351 = ORIENTED_EDGE('',*,*,#8189,.F.) ;
#11352 = ORIENTED_EDGE('',*,*,#8188,.F.) ;
#11353 = ORIENTED_EDGE('',*,*,#8190,.T.) ;
#11354 = ORIENTED_EDGE('',*,*,#8184,.F.) ;
#11355 = ORIENTED_EDGE('',*,*,#8181,.T.) ;
#11356 = ORIENTED_EDGE('',*,*,#8185,.F.) ;
#11357 = ORIENTED_EDGE('',*,*,#8190,.F.) ;
#11358 = ORIENTED_EDGE('',*,*,#8187,.F.) ;
#11359 = ORIENTED_EDGE('',*,*,#8191,.F.) ;
#11360 = ORIENTED_EDGE('',*,*,#8192,.T.) ;
#11361 = ORIENTED_EDGE('',*,*,#8130,.T.) ;
#11362 = ORIENTED_EDGE('',*,*,#8122,.T.) ;
#11363 = ORIENTED_EDGE('',*,*,#8117,.T.) ;
#11364 = ORIENTED_EDGE('',*,*,#8193,.T.) ;
#11365 = ORIENTED_EDGE('',*,*,#8194,.F.) ;
#11366 = ORIENTED_EDGE('',*,*,#8193,.F.) ;
#11367 = ORIENTED_EDGE('',*,*,#8121,.T.) ;
#11368 = ORIENTED_EDGE('',*,*,#8125,.T.) ;
#11369 = ORIENTED_EDGE('',*,*,#8128,.T.) ;
#11370 = ORIENTED_EDGE('',*,*,#8192,.F.) ;
#11371 = ORIENTED_EDGE('',*,*,#8073,.T.) ;
#11372 = ORIENTED_EDGE('',*,*,#8069,.T.) ;
#11373 = ORIENTED_EDGE('',*,*,#8076,.T.) ;
#11374 = ORIENTED_EDGE('',*,*,#8079,.T.) ;
#11375 = ORIENTED_EDGE('',*,*,#8085,.T.) ;
#11376 = ORIENTED_EDGE('',*,*,#8081,.T.) ;
#11377 = ORIENTED_EDGE('',*,*,#8088,.T.) ;
#11378 = ORIENTED_EDGE('',*,*,#8091,.T.) ;
#11379 = ORIENTED_EDGE('',*,*,#8097,.T.) ;
#11380 = ORIENTED_EDGE('',*,*,#8093,.T.) ;
#11381 = ORIENTED_EDGE('',*,*,#8100,.T.) ;
#11382 = ORIENTED_EDGE('',*,*,#8103,.T.) ;
#11383 = ORIENTED_EDGE('',*,*,#8109,.T.) ;
#11384 = ORIENTED_EDGE('',*,*,#8105,.T.) ;
#11385 = ORIENTED_EDGE('',*,*,#8112,.T.) ;
#11386 = ORIENTED_EDGE('',*,*,#8115,.T.) ;
#11387 = ORIENTED_EDGE('',*,*,#8135,.T.) ;
#11388 = ORIENTED_EDGE('',*,*,#8131,.T.) ;
#11389 = ORIENTED_EDGE('',*,*,#8138,.T.) ;
#11390 = ORIENTED_EDGE('',*,*,#8141,.T.) ;
#11391 = ORIENTED_EDGE('',*,*,#8147,.T.) ;
#11392 = ORIENTED_EDGE('',*,*,#8143,.T.) ;
#11393 = ORIENTED_EDGE('',*,*,#8150,.T.) ;
#11394 = ORIENTED_EDGE('',*,*,#8153,.T.) ;
#11395 = ORIENTED_EDGE('',*,*,#8159,.T.) ;
#11396 = ORIENTED_EDGE('',*,*,#8155,.T.) ;
#11397 = ORIENTED_EDGE('',*,*,#8162,.T.) ;
#11398 = ORIENTED_EDGE('',*,*,#8165,.T.) ;
#11399 = ORIENTED_EDGE('',*,*,#8171,.T.) ;
#11400 = ORIENTED_EDGE('',*,*,#8167,.T.) ;
#11401 = ORIENTED_EDGE('',*,*,#8174,.T.) ;
#11402 = ORIENTED_EDGE('',*,*,#8177,.T.) ;
#11403 = ORIENTED_EDGE('',*,*,#8183,.T.) ;
#11404 = ORIENTED_EDGE('',*,*,#8179,.T.) ;
#11405 = ORIENTED_EDGE('',*,*,#8186,.T.) ;
#11406 = ORIENTED_EDGE('',*,*,#8189,.T.) ;
#11407 = ORIENTED_EDGE('',*,*,#8194,.T.) ;
#11408 = ORIENTED_EDGE('',*,*,#8066,.T.) ;
#11409 = ORIENTED_EDGE('',*,*,#8191,.T.) ;
#11410 = ORIENTED_EDGE('',*,*,#8065,.T.) ;
#11411 = ORIENTED_EDGE('',*,*,#8195,.F.) ;
#11412 = ORIENTED_EDGE('',*,*,#8196,.T.) ;
#11413 = ORIENTED_EDGE('',*,*,#8197,.F.) ;
#11414 = ORIENTED_EDGE('',*,*,#8196,.F.) ;
#11415 = ORIENTED_EDGE('',*,*,#8198,.F.) ;
#11416 = ORIENTED_EDGE('',*,*,#8199,.T.) ;
#11417 = ORIENTED_EDGE('',*,*,#8200,.F.) ;
#11418 = ORIENTED_EDGE('',*,*,#8199,.F.) ;
#11419 = ORIENTED_EDGE('',*,*,#8200,.T.) ;
#11420 = ORIENTED_EDGE('',*,*,#8195,.T.) ;
#11421 = ORIENTED_EDGE('',*,*,#8198,.T.) ;
#11422 = ORIENTED_EDGE('',*,*,#8197,.T.) ;
#11423 = ORIENTED_EDGE('',*,*,#8201,.F.) ;
#11424 = ORIENTED_EDGE('',*,*,#8202,.T.) ;
#11425 = ORIENTED_EDGE('',*,*,#8203,.F.) ;
#11426 = ORIENTED_EDGE('',*,*,#8204,.T.) ;
#11427 = ORIENTED_EDGE('',*,*,#8205,.F.) ;
#11428 = ORIENTED_EDGE('',*,*,#8206,.T.) ;
#11429 = ORIENTED_EDGE('',*,*,#8202,.F.) ;
#11430 = ORIENTED_EDGE('',*,*,#8207,.F.) ;
#11431 = ORIENTED_EDGE('',*,*,#8206,.F.) ;
#11432 = ORIENTED_EDGE('',*,*,#8208,.F.) ;
#11433 = ORIENTED_EDGE('',*,*,#8204,.F.) ;
#11434 = ORIENTED_EDGE('',*,*,#8209,.F.) ;
#11435 = ORIENTED_EDGE('',*,*,#8210,.T.) ;
#11436 = ORIENTED_EDGE('',*,*,#8211,.F.) ;
#11437 = ORIENTED_EDGE('',*,*,#8210,.F.) ;
#11438 = ORIENTED_EDGE('',*,*,#8212,.F.) ;
#11439 = ORIENTED_EDGE('',*,*,#8205,.T.) ;
#11440 = ORIENTED_EDGE('',*,*,#8211,.T.) ;
#11441 = ORIENTED_EDGE('',*,*,#8207,.T.) ;
#11442 = ORIENTED_EDGE('',*,*,#8213,.F.) ;
#11443 = ORIENTED_EDGE('',*,*,#8214,.T.) ;
#11444 = ORIENTED_EDGE('',*,*,#8215,.F.) ;
#11445 = ORIENTED_EDGE('',*,*,#8216,.F.) ;
#11446 = ORIENTED_EDGE('',*,*,#8217,.F.) ;
#11447 = ORIENTED_EDGE('',*,*,#8214,.F.) ;
#11448 = ORIENTED_EDGE('',*,*,#8212,.T.) ;
#11449 = ORIENTED_EDGE('',*,*,#8218,.F.) ;
#11450 = ORIENTED_EDGE('',*,*,#8219,.T.) ;
#11451 = ORIENTED_EDGE('',*,*,#8216,.T.) ;
#11452 = ORIENTED_EDGE('',*,*,#8220,.T.) ;
#11453 = ORIENTED_EDGE('',*,*,#8221,.T.) ;
#11454 = ORIENTED_EDGE('',*,*,#8222,.T.) ;
#11455 = ORIENTED_EDGE('',*,*,#8222,.F.) ;
#11456 = ORIENTED_EDGE('',*,*,#8223,.T.) ;
#11457 = ORIENTED_EDGE('',*,*,#8224,.T.) ;
#11458 = ORIENTED_EDGE('',*,*,#8225,.T.) ;
#11459 = ORIENTED_EDGE('',*,*,#8226,.T.) ;
#11460 = ORIENTED_EDGE('',*,*,#8227,.T.) ;
#11461 = ORIENTED_EDGE('',*,*,#8208,.T.) ;
#11462 = ORIENTED_EDGE('',*,*,#8218,.T.) ;
#11463 = ORIENTED_EDGE('',*,*,#8209,.T.) ;
#11464 = ORIENTED_EDGE('',*,*,#8203,.T.) ;
#11465 = ORIENTED_EDGE('',*,*,#8213,.T.) ;
#11466 = ORIENTED_EDGE('',*,*,#8201,.T.) ;
#11467 = ORIENTED_EDGE('',*,*,#8215,.T.) ;
#11468 = ORIENTED_EDGE('',*,*,#8228,.T.) ;
#11469 = ORIENTED_EDGE('',*,*,#8229,.F.) ;
#11470 = ORIENTED_EDGE('',*,*,#8223,.F.) ;
#11471 = ORIENTED_EDGE('',*,*,#8221,.F.) ;
#11472 = ORIENTED_EDGE('',*,*,#8230,.F.) ;
#11473 = ORIENTED_EDGE('',*,*,#8228,.F.) ;
#11474 = ORIENTED_EDGE('',*,*,#8217,.T.) ;
#11475 = ORIENTED_EDGE('',*,*,#8220,.F.) ;
#11476 = ORIENTED_EDGE('',*,*,#8229,.T.) ;
#11477 = ORIENTED_EDGE('',*,*,#8230,.T.) ;
#11478 = ORIENTED_EDGE('',*,*,#8225,.F.) ;
#11479 = ORIENTED_EDGE('',*,*,#8231,.T.) ;
#11480 = ORIENTED_EDGE('',*,*,#8226,.F.) ;
#11481 = ORIENTED_EDGE('',*,*,#8232,.F.) ;
#11482 = ORIENTED_EDGE('',*,*,#8231,.F.) ;
#11483 = ORIENTED_EDGE('',*,*,#8224,.F.) ;
#11484 = ORIENTED_EDGE('',*,*,#8219,.F.) ;
#11485 = ORIENTED_EDGE('',*,*,#8233,.T.) ;
#11486 = ORIENTED_EDGE('',*,*,#8234,.F.) ;
#11487 = ORIENTED_EDGE('',*,*,#8233,.F.) ;
#11488 = ORIENTED_EDGE('',*,*,#8235,.F.) ;
#11489 = ORIENTED_EDGE('',*,*,#8236,.T.) ;
#11490 = ORIENTED_EDGE('',*,*,#8232,.T.) ;
#11491 = ORIENTED_EDGE('',*,*,#8227,.F.) ;
#11492 = ORIENTED_EDGE('',*,*,#8236,.F.) ;
#11493 = ORIENTED_EDGE('',*,*,#8235,.T.) ;
#11494 = ORIENTED_EDGE('',*,*,#8234,.T.) ;
#11495 = ORIENTED_EDGE('',*,*,#8237,.F.) ;
#11496 = ORIENTED_EDGE('',*,*,#8238,.F.) ;
#11497 = ORIENTED_EDGE('',*,*,#8239,.F.) ;
#11498 = ORIENTED_EDGE('',*,*,#8240,.F.) ;
#11499 = ORIENTED_EDGE('',*,*,#8241,.F.) ;
#11500 = ORIENTED_EDGE('',*,*,#8242,.F.) ;
#11501 = ORIENTED_EDGE('',*,*,#8243,.F.) ;
#11502 = ORIENTED_EDGE('',*,*,#8244,.F.) ;
#11503 = ORIENTED_EDGE('',*,*,#8245,.F.) ;
#11504 = ORIENTED_EDGE('',*,*,#8246,.F.) ;
#11505 = ORIENTED_EDGE('',*,*,#8247,.T.) ;
#11506 = ORIENTED_EDGE('',*,*,#8248,.F.) ;
#11507 = ORIENTED_EDGE('',*,*,#8239,.T.) ;
#11508 = ORIENTED_EDGE('',*,*,#8249,.F.) ;
#11509 = ORIENTED_EDGE('',*,*,#8247,.F.) ;
#11510 = ORIENTED_EDGE('',*,*,#8250,.F.) ;
#11511 = ORIENTED_EDGE('',*,*,#8251,.T.) ;
#11512 = ORIENTED_EDGE('',*,*,#8248,.T.) ;
#11513 = ORIENTED_EDGE('',*,*,#8249,.T.) ;
#11514 = ORIENTED_EDGE('',*,*,#8238,.T.) ;
#11515 = ORIENTED_EDGE('',*,*,#8252,.T.) ;
#11516 = ORIENTED_EDGE('',*,*,#8244,.T.) ;
#11517 = ORIENTED_EDGE('',*,*,#8241,.T.) ;
#11518 = ORIENTED_EDGE('',*,*,#8252,.F.) ;
#11519 = ORIENTED_EDGE('',*,*,#8243,.T.) ;
#11520 = ORIENTED_EDGE('',*,*,#8253,.F.) ;
#11521 = ORIENTED_EDGE('',*,*,#8237,.T.) ;
#11522 = ORIENTED_EDGE('',*,*,#8254,.F.) ;
#11523 = ORIENTED_EDGE('',*,*,#8245,.T.) ;
#11524 = ORIENTED_EDGE('',*,*,#8251,.F.) ;
#11525 = ORIENTED_EDGE('',*,*,#8240,.T.) ;
#11526 = ORIENTED_EDGE('',*,*,#8250,.T.) ;
#11527 = ORIENTED_EDGE('',*,*,#8246,.T.) ;
#11528 = ORIENTED_EDGE('',*,*,#8254,.T.) ;
#11529 = ORIENTED_EDGE('',*,*,#8253,.T.) ;
#11530 = ORIENTED_EDGE('',*,*,#8242,.T.) ;
#11531 = ORIENTED_EDGE('',*,*,#8255,.F.) ;
#11532 = ORIENTED_EDGE('',*,*,#8256,.T.) ;
#11533 = ORIENTED_EDGE('',*,*,#8257,.T.) ;
#11534 = ORIENTED_EDGE('',*,*,#8258,.T.) ;
#11535 = ORIENTED_EDGE('',*,*,#8259,.F.) ;
#11536 = ORIENTED_EDGE('',*,*,#8260,.F.) ;
#11537 = ORIENTED_EDGE('',*,*,#8261,.F.) ;
#11538 = ORIENTED_EDGE('',*,*,#8262,.T.) ;
#11539 = ORIENTED_EDGE('',*,*,#8263,.F.) ;
#11540 = ORIENTED_EDGE('',*,*,#8264,.T.) ;
#11541 = ORIENTED_EDGE('',*,*,#8265,.T.) ;
#11542 = ORIENTED_EDGE('',*,*,#8266,.T.) ;
#11543 = ORIENTED_EDGE('',*,*,#8267,.T.) ;
#11544 = ORIENTED_EDGE('',*,*,#8265,.F.) ;
#11545 = ORIENTED_EDGE('',*,*,#8268,.F.) ;
#11546 = ORIENTED_EDGE('',*,*,#8257,.F.) ;
#11547 = ORIENTED_EDGE('',*,*,#8263,.T.) ;
#11548 = ORIENTED_EDGE('',*,*,#8269,.F.) ;
#11549 = ORIENTED_EDGE('',*,*,#8255,.T.) ;
#11550 = ORIENTED_EDGE('',*,*,#8270,.F.) ;
#11551 = ORIENTED_EDGE('',*,*,#8259,.T.) ;
#11552 = ORIENTED_EDGE('',*,*,#8271,.F.) ;
#11553 = ORIENTED_EDGE('',*,*,#8261,.T.) ;
#11554 = ORIENTED_EDGE('',*,*,#8272,.F.) ;
#11555 = ORIENTED_EDGE('',*,*,#8269,.T.) ;
#11556 = ORIENTED_EDGE('',*,*,#8266,.F.) ;
#11557 = ORIENTED_EDGE('',*,*,#8267,.F.) ;
#11558 = ORIENTED_EDGE('',*,*,#8256,.F.) ;
#11559 = ORIENTED_EDGE('',*,*,#8272,.T.) ;
#11560 = ORIENTED_EDGE('',*,*,#8260,.T.) ;
#11561 = ORIENTED_EDGE('',*,*,#8270,.T.) ;
#11562 = ORIENTED_EDGE('',*,*,#8258,.F.) ;
#11563 = ORIENTED_EDGE('',*,*,#8268,.T.) ;
#11564 = ORIENTED_EDGE('',*,*,#8264,.F.) ;
#11565 = ORIENTED_EDGE('',*,*,#8271,.T.) ;
#11566 = ORIENTED_EDGE('',*,*,#8262,.F.) ;
#11567 = ORIENTED_EDGE('',*,*,#8273,.F.) ;
#11568 = ORIENTED_EDGE('',*,*,#8274,.F.) ;
#11569 = ORIENTED_EDGE('',*,*,#8275,.T.) ;
#11570 = ORIENTED_EDGE('',*,*,#8276,.F.) ;
#11571 = ORIENTED_EDGE('',*,*,#8277,.F.) ;
#11572 = ORIENTED_EDGE('',*,*,#8278,.F.) ;
#11573 = ORIENTED_EDGE('',*,*,#8275,.F.) ;
#11574 = ORIENTED_EDGE('',*,*,#8279,.F.) ;
#11575 = ORIENTED_EDGE('',*,*,#8280,.F.) ;
#11576 = ORIENTED_EDGE('',*,*,#8281,.T.) ;
#11577 = ORIENTED_EDGE('',*,*,#8274,.T.) ;
#11578 = ORIENTED_EDGE('',*,*,#8273,.T.) ;
#11579 = ORIENTED_EDGE('',*,*,#8282,.T.) ;
#11580 = ORIENTED_EDGE('',*,*,#8283,.F.) ;
#11581 = ORIENTED_EDGE('',*,*,#8282,.F.) ;
#11582 = ORIENTED_EDGE('',*,*,#8279,.T.) ;
#11583 = ORIENTED_EDGE('',*,*,#8281,.F.) ;
#11584 = ORIENTED_EDGE('',*,*,#8284,.F.) ;
#11585 = ORIENTED_EDGE('',*,*,#8285,.T.) ;
#11586 = ORIENTED_EDGE('',*,*,#8277,.T.) ;
#11587 = ORIENTED_EDGE('',*,*,#8276,.T.) ;
#11588 = ORIENTED_EDGE('',*,*,#8286,.T.) ;
#11589 = ORIENTED_EDGE('',*,*,#8287,.F.) ;
#11590 = ORIENTED_EDGE('',*,*,#8286,.F.) ;
#11591 = ORIENTED_EDGE('',*,*,#8278,.T.) ;
#11592 = ORIENTED_EDGE('',*,*,#8285,.F.) ;
#11593 = ORIENTED_EDGE('',*,*,#8287,.T.) ;
#11594 = ORIENTED_EDGE('',*,*,#8280,.T.) ;
#11595 = ORIENTED_EDGE('',*,*,#8284,.T.) ;
#11596 = ORIENTED_EDGE('',*,*,#8283,.T.) ;
#11597 = ORIENTED_EDGE('',*,*,#8288,.F.) ;
#11598 = ORIENTED_EDGE('',*,*,#8289,.F.) ;
#11599 = ORIENTED_EDGE('',*,*,#8290,.F.) ;
#11600 = ORIENTED_EDGE('',*,*,#8291,.F.) ;
#11601 = ORIENTED_EDGE('',*,*,#8292,.F.) ;
#11602 = ORIENTED_EDGE('',*,*,#8291,.T.) ;
#11603 = ORIENTED_EDGE('',*,*,#8293,.F.) ;
#11604 = ORIENTED_EDGE('',*,*,#8294,.F.) ;
#11605 = ORIENTED_EDGE('',*,*,#8295,.T.) ;
#11606 = ORIENTED_EDGE('',*,*,#8296,.F.) ;
#11607 = ORIENTED_EDGE('',*,*,#8297,.F.) ;
#11608 = ORIENTED_EDGE('',*,*,#8298,.T.) ;
#11609 = ORIENTED_EDGE('',*,*,#8299,.F.) ;
#11610 = ORIENTED_EDGE('',*,*,#8300,.F.) ;
#11611 = ORIENTED_EDGE('',*,*,#8289,.T.) ;
#11612 = ORIENTED_EDGE('',*,*,#8301,.F.) ;
#11613 = ORIENTED_EDGE('',*,*,#8302,.F.) ;
#11614 = ORIENTED_EDGE('',*,*,#8295,.F.) ;
#11615 = ORIENTED_EDGE('',*,*,#8303,.F.) ;
#11616 = ORIENTED_EDGE('',*,*,#8298,.F.) ;
#11617 = ORIENTED_EDGE('',*,*,#8304,.F.) ;
#11618 = ORIENTED_EDGE('',*,*,#8305,.T.) ;
#11619 = ORIENTED_EDGE('',*,*,#8296,.T.) ;
#11620 = ORIENTED_EDGE('',*,*,#8302,.T.) ;
#11621 = ORIENTED_EDGE('',*,*,#8297,.T.) ;
#11622 = ORIENTED_EDGE('',*,*,#8306,.T.) ;
#11623 = ORIENTED_EDGE('',*,*,#8307,.F.) ;
#11624 = ORIENTED_EDGE('',*,*,#8306,.F.) ;
#11625 = ORIENTED_EDGE('',*,*,#8301,.T.) ;
#11626 = ORIENTED_EDGE('',*,*,#8288,.T.) ;
#11627 = ORIENTED_EDGE('',*,*,#8292,.T.) ;
#11628 = ORIENTED_EDGE('',*,*,#8305,.F.) ;
#11629 = ORIENTED_EDGE('',*,*,#8308,.F.) ;
#11630 = ORIENTED_EDGE('',*,*,#8309,.T.) ;
#11631 = ORIENTED_EDGE('',*,*,#8310,.T.) ;
#11632 = ORIENTED_EDGE('',*,*,#8309,.F.) ;
#11633 = ORIENTED_EDGE('',*,*,#8308,.T.) ;
#11634 = ORIENTED_EDGE('',*,*,#8307,.T.) ;
#11635 = ORIENTED_EDGE('',*,*,#8310,.F.) ;
#11636 = ORIENTED_EDGE('',*,*,#8311,.T.) ;
#11637 = ORIENTED_EDGE('',*,*,#8299,.T.) ;
#11638 = ORIENTED_EDGE('',*,*,#8303,.T.) ;
#11639 = ORIENTED_EDGE('',*,*,#8294,.T.) ;
#11640 = ORIENTED_EDGE('',*,*,#8312,.T.) ;
#11641 = ORIENTED_EDGE('',*,*,#8313,.T.) ;
#11642 = ORIENTED_EDGE('',*,*,#8312,.F.) ;
#11643 = ORIENTED_EDGE('',*,*,#8293,.T.) ;
#11644 = ORIENTED_EDGE('',*,*,#8290,.T.) ;
#11645 = ORIENTED_EDGE('',*,*,#8300,.T.) ;
#11646 = ORIENTED_EDGE('',*,*,#8311,.F.) ;
#11647 = ORIENTED_EDGE('',*,*,#8313,.F.) ;
#11648 = ORIENTED_EDGE('',*,*,#8314,.T.) ;
#11649 = ORIENTED_EDGE('',*,*,#8315,.F.) ;
#11650 = ORIENTED_EDGE('',*,*,#8314,.F.) ;
#11651 = ORIENTED_EDGE('',*,*,#8315,.T.) ;
#11652 = ORIENTED_EDGE('',*,*,#8304,.T.) ;
#11653 = ORIENTED_EDGE('',*,*,#8316,.F.) ;
#11654 = ORIENTED_EDGE('',*,*,#8317,.T.) ;
#11655 = ORIENTED_EDGE('',*,*,#8318,.F.) ;
#11656 = ORIENTED_EDGE('',*,*,#8317,.F.) ;
#11657 = ORIENTED_EDGE('',*,*,#8319,.F.) ;
#11658 = ORIENTED_EDGE('',*,*,#8320,.T.) ;
#11659 = ORIENTED_EDGE('',*,*,#8321,.F.) ;
#11660 = ORIENTED_EDGE('',*,*,#8320,.F.) ;
#11661 = ORIENTED_EDGE('',*,*,#8321,.T.) ;
#11662 = ORIENTED_EDGE('',*,*,#8316,.T.) ;
#11663 = ORIENTED_EDGE('',*,*,#8319,.T.) ;
#11664 = ORIENTED_EDGE('',*,*,#8318,.T.) ;
#11665 = ORIENTED_EDGE('',*,*,#8322,.F.) ;
#11666 = ORIENTED_EDGE('',*,*,#8323,.T.) ;
#11667 = ORIENTED_EDGE('',*,*,#8324,.F.) ;
#11668 = ORIENTED_EDGE('',*,*,#8323,.F.) ;
#11669 = ORIENTED_EDGE('',*,*,#8325,.F.) ;
#11670 = ORIENTED_EDGE('',*,*,#8326,.T.) ;
#11671 = ORIENTED_EDGE('',*,*,#8327,.F.) ;
#11672 = ORIENTED_EDGE('',*,*,#8326,.F.) ;
#11673 = ORIENTED_EDGE('',*,*,#8328,.F.) ;
#11674 = ORIENTED_EDGE('',*,*,#8329,.T.) ;
#11675 = ORIENTED_EDGE('',*,*,#8330,.F.) ;
#11676 = ORIENTED_EDGE('',*,*,#8329,.F.) ;
#11677 = ORIENTED_EDGE('',*,*,#8331,.F.) ;
#11678 = ORIENTED_EDGE('',*,*,#8332,.T.) ;
#11679 = ORIENTED_EDGE('',*,*,#8333,.F.) ;
#11680 = ORIENTED_EDGE('',*,*,#8332,.F.) ;
#11681 = ORIENTED_EDGE('',*,*,#8334,.F.) ;
#11682 = ORIENTED_EDGE('',*,*,#8335,.T.) ;
#11683 = ORIENTED_EDGE('',*,*,#8336,.F.) ;
#11684 = ORIENTED_EDGE('',*,*,#8335,.F.) ;
#11685 = ORIENTED_EDGE('',*,*,#8337,.F.) ;
#11686 = ORIENTED_EDGE('',*,*,#8338,.T.) ;
#11687 = ORIENTED_EDGE('',*,*,#8339,.F.) ;
#11688 = ORIENTED_EDGE('',*,*,#8338,.F.) ;
#11689 = ORIENTED_EDGE('',*,*,#8339,.T.) ;
#11690 = ORIENTED_EDGE('',*,*,#8322,.T.) ;
#11691 = ORIENTED_EDGE('',*,*,#8325,.T.) ;
#11692 = ORIENTED_EDGE('',*,*,#8328,.T.) ;
#11693 = ORIENTED_EDGE('',*,*,#8331,.T.) ;
#11694 = ORIENTED_EDGE('',*,*,#8334,.T.) ;
#11695 = ORIENTED_EDGE('',*,*,#8337,.T.) ;
#11696 = ORIENTED_EDGE('',*,*,#8324,.T.) ;
#11697 = ORIENTED_EDGE('',*,*,#8327,.T.) ;
#11698 = ORIENTED_EDGE('',*,*,#8330,.T.) ;
#11699 = ORIENTED_EDGE('',*,*,#8333,.T.) ;
#11700 = ORIENTED_EDGE('',*,*,#8336,.T.) ;
#11701 = ORIENTED_EDGE('',*,*,#8340,.F.) ;
#11702 = ORIENTED_EDGE('',*,*,#8341,.T.) ;
#11703 = ORIENTED_EDGE('',*,*,#8342,.F.) ;
#11704 = ORIENTED_EDGE('',*,*,#8341,.F.) ;
#11705 = ORIENTED_EDGE('',*,*,#8343,.F.) ;
#11706 = ORIENTED_EDGE('',*,*,#8344,.T.) ;
#11707 = ORIENTED_EDGE('',*,*,#8345,.F.) ;
#11708 = ORIENTED_EDGE('',*,*,#8344,.F.) ;
#11709 = ORIENTED_EDGE('',*,*,#8346,.F.) ;
#11710 = ORIENTED_EDGE('',*,*,#8347,.T.) ;
#11711 = ORIENTED_EDGE('',*,*,#8348,.F.) ;
#11712 = ORIENTED_EDGE('',*,*,#8347,.F.) ;
#11713 = ORIENTED_EDGE('',*,*,#8349,.F.) ;
#11714 = ORIENTED_EDGE('',*,*,#8350,.T.) ;
#11715 = ORIENTED_EDGE('',*,*,#8351,.F.) ;
#11716 = ORIENTED_EDGE('',*,*,#8350,.F.) ;
#11717 = ORIENTED_EDGE('',*,*,#8352,.F.) ;
#11718 = ORIENTED_EDGE('',*,*,#8353,.T.) ;
#11719 = ORIENTED_EDGE('',*,*,#8354,.F.) ;
#11720 = ORIENTED_EDGE('',*,*,#8353,.F.) ;
#11721 = ORIENTED_EDGE('',*,*,#8355,.F.) ;
#11722 = ORIENTED_EDGE('',*,*,#8356,.T.) ;
#11723 = ORIENTED_EDGE('',*,*,#8357,.F.) ;
#11724 = ORIENTED_EDGE('',*,*,#8356,.F.) ;
#11725 = ORIENTED_EDGE('',*,*,#8357,.T.) ;
#11726 = ORIENTED_EDGE('',*,*,#8340,.T.) ;
#11727 = ORIENTED_EDGE('',*,*,#8343,.T.) ;
#11728 = ORIENTED_EDGE('',*,*,#8346,.T.) ;
#11729 = ORIENTED_EDGE('',*,*,#8349,.T.) ;
#11730 = ORIENTED_EDGE('',*,*,#8352,.T.) ;
#11731 = ORIENTED_EDGE('',*,*,#8355,.T.) ;
#11732 = ORIENTED_EDGE('',*,*,#8342,.T.) ;
#11733 = ORIENTED_EDGE('',*,*,#8345,.T.) ;
#11734 = ORIENTED_EDGE('',*,*,#8348,.T.) ;
#11735 = ORIENTED_EDGE('',*,*,#8351,.T.) ;
#11736 = ORIENTED_EDGE('',*,*,#8354,.T.) ;
#11737 = ORIENTED_EDGE('',*,*,#8358,.F.) ;
#11738 = ORIENTED_EDGE('',*,*,#8359,.F.) ;
#11739 = ORIENTED_EDGE('',*,*,#8360,.F.) ;
#11740 = ORIENTED_EDGE('',*,*,#8361,.T.) ;
#11741 = ORIENTED_EDGE('',*,*,#8362,.F.) ;
#11742 = ORIENTED_EDGE('',*,*,#8361,.F.) ;
#11743 = ORIENTED_EDGE('',*,*,#8363,.F.) ;
#11744 = ORIENTED_EDGE('',*,*,#8359,.T.) ;
#11745 = ORIENTED_EDGE('',*,*,#8364,.F.) ;
#11746 = ORIENTED_EDGE('',*,*,#8365,.F.) ;
#11747 = ORIENTED_EDGE('',*,*,#8366,.F.) ;
#11748 = ORIENTED_EDGE('',*,*,#8367,.T.) ;
#11749 = ORIENTED_EDGE('',*,*,#8368,.F.) ;
#11750 = ORIENTED_EDGE('',*,*,#8367,.F.) ;
#11751 = ORIENTED_EDGE('',*,*,#8369,.F.) ;
#11752 = ORIENTED_EDGE('',*,*,#8365,.T.) ;
#11753 = ORIENTED_EDGE('',*,*,#8370,.F.) ;
#11754 = ORIENTED_EDGE('',*,*,#8371,.T.) ;
#11755 = ORIENTED_EDGE('',*,*,#8372,.T.) ;
#11756 = ORIENTED_EDGE('',*,*,#8373,.T.) ;
#11757 = ORIENTED_EDGE('',*,*,#8368,.T.) ;
#11758 = ORIENTED_EDGE('',*,*,#8374,.F.) ;
#11759 = ORIENTED_EDGE('',*,*,#8375,.T.) ;
#11760 = ORIENTED_EDGE('',*,*,#8376,.T.) ;
#11761 = ORIENTED_EDGE('',*,*,#8377,.T.) ;
#11762 = ORIENTED_EDGE('',*,*,#8362,.T.) ;
#11763 = ORIENTED_EDGE('',*,*,#8378,.T.) ;
#11764 = ORIENTED_EDGE('',*,*,#8379,.T.) ;
#11765 = ORIENTED_EDGE('',*,*,#8380,.T.) ;
#11766 = ORIENTED_EDGE('',*,*,#8381,.T.) ;
#11767 = ORIENTED_EDGE('',*,*,#8360,.T.) ;
#11768 = ORIENTED_EDGE('',*,*,#8366,.T.) ;
#11769 = ORIENTED_EDGE('',*,*,#8382,.T.) ;
#11770 = ORIENTED_EDGE('',*,*,#8379,.F.) ;
#11771 = ORIENTED_EDGE('',*,*,#8383,.F.) ;
#11772 = ORIENTED_EDGE('',*,*,#8372,.F.) ;
#11773 = ORIENTED_EDGE('',*,*,#8384,.T.) ;
#11774 = ORIENTED_EDGE('',*,*,#8381,.F.) ;
#11775 = ORIENTED_EDGE('',*,*,#8385,.F.) ;
#11776 = ORIENTED_EDGE('',*,*,#8376,.F.) ;
#11777 = ORIENTED_EDGE('',*,*,#8386,.T.) ;
#11778 = ORIENTED_EDGE('',*,*,#8377,.F.) ;
#11779 = ORIENTED_EDGE('',*,*,#8385,.T.) ;
#11780 = ORIENTED_EDGE('',*,*,#8380,.F.) ;
#11781 = ORIENTED_EDGE('',*,*,#8382,.F.) ;
#11782 = ORIENTED_EDGE('',*,*,#8371,.F.) ;
#11783 = ORIENTED_EDGE('',*,*,#8387,.T.) ;
#11784 = ORIENTED_EDGE('',*,*,#8374,.T.) ;
#11785 = ORIENTED_EDGE('',*,*,#8386,.F.) ;
#11786 = ORIENTED_EDGE('',*,*,#8370,.T.) ;
#11787 = ORIENTED_EDGE('',*,*,#8388,.F.) ;
#11788 = ORIENTED_EDGE('',*,*,#8363,.T.) ;
#11789 = ORIENTED_EDGE('',*,*,#8358,.T.) ;
#11790 = ORIENTED_EDGE('',*,*,#8369,.T.) ;
#11791 = ORIENTED_EDGE('',*,*,#8364,.T.) ;
#11792 = ORIENTED_EDGE('',*,*,#8387,.F.) ;
#11793 = ORIENTED_EDGE('',*,*,#8389,.T.) ;
#11794 = ORIENTED_EDGE('',*,*,#8390,.F.) ;
#11795 = ORIENTED_EDGE('',*,*,#8389,.F.) ;
#11796 = ORIENTED_EDGE('',*,*,#8388,.T.) ;
#11797 = ORIENTED_EDGE('',*,*,#8373,.F.) ;
#11798 = ORIENTED_EDGE('',*,*,#8383,.T.) ;
#11799 = ORIENTED_EDGE('',*,*,#8378,.F.) ;
#11800 = ORIENTED_EDGE('',*,*,#8384,.F.) ;
#11801 = ORIENTED_EDGE('',*,*,#8375,.F.) ;
#11802 = ORIENTED_EDGE('',*,*,#8390,.T.) ;
#11803 = ORIENTED_EDGE('',*,*,#8391,.F.) ;
#11804 = ORIENTED_EDGE('',*,*,#8392,.T.) ;
#11805 = ORIENTED_EDGE('',*,*,#8393,.F.) ;
#11806 = ORIENTED_EDGE('',*,*,#8392,.F.) ;
#11807 = ORIENTED_EDGE('',*,*,#8391,.T.) ;
#11808 = ORIENTED_EDGE('',*,*,#8394,.F.) ;
#11809 = ORIENTED_EDGE('',*,*,#8395,.T.) ;
#11810 = ORIENTED_EDGE('',*,*,#8396,.F.) ;
#11811 = ORIENTED_EDGE('',*,*,#8395,.F.) ;
#11812 = ORIENTED_EDGE('',*,*,#8396,.T.) ;
#11813 = ORIENTED_EDGE('',*,*,#8394,.T.) ;
#11814 = ORIENTED_EDGE('',*,*,#8393,.T.) ;
#11815 = ORIENTED_EDGE('',*,*,#8397,.F.) ;
#11816 = ORIENTED_EDGE('',*,*,#8398,.T.) ;
#11817 = ORIENTED_EDGE('',*,*,#8399,.F.) ;
#11818 = ORIENTED_EDGE('',*,*,#8398,.F.) ;
#11819 = ORIENTED_EDGE('',*,*,#8400,.F.) ;
#11820 = ORIENTED_EDGE('',*,*,#8401,.T.) ;
#11821 = ORIENTED_EDGE('',*,*,#8402,.F.) ;
#11822 = ORIENTED_EDGE('',*,*,#8401,.F.) ;
#11823 = ORIENTED_EDGE('',*,*,#8402,.T.) ;
#11824 = ORIENTED_EDGE('',*,*,#8397,.T.) ;
#11825 = ORIENTED_EDGE('',*,*,#8400,.T.) ;
#11826 = ORIENTED_EDGE('',*,*,#8399,.T.) ;
#11827 = ORIENTED_EDGE('',*,*,#8403,.F.) ;
#11828 = ORIENTED_EDGE('',*,*,#8404,.T.) ;
#11829 = ORIENTED_EDGE('',*,*,#8405,.F.) ;
#11830 = ORIENTED_EDGE('',*,*,#8404,.F.) ;
#11831 = ORIENTED_EDGE('',*,*,#8406,.F.) ;
#11832 = ORIENTED_EDGE('',*,*,#8407,.T.) ;
#11833 = ORIENTED_EDGE('',*,*,#8408,.F.) ;
#11834 = ORIENTED_EDGE('',*,*,#8409,.T.) ;
#11835 = ORIENTED_EDGE('',*,*,#8410,.F.) ;
#11836 = ORIENTED_EDGE('',*,*,#8411,.T.) ;
#11837 = ORIENTED_EDGE('',*,*,#8412,.F.) ;
#11838 = ORIENTED_EDGE('',*,*,#8413,.T.) ;
#11839 = ORIENTED_EDGE('',*,*,#8407,.F.) ;
#11840 = ORIENTED_EDGE('',*,*,#8414,.F.) ;
#11841 = ORIENTED_EDGE('',*,*,#8415,.F.) ;
#11842 = ORIENTED_EDGE('',*,*,#8411,.F.) ;
#11843 = ORIENTED_EDGE('',*,*,#8416,.F.) ;
#11844 = ORIENTED_EDGE('',*,*,#8417,.F.) ;
#11845 = ORIENTED_EDGE('',*,*,#8403,.T.) ;
#11846 = ORIENTED_EDGE('',*,*,#8418,.F.) ;
#11847 = ORIENTED_EDGE('',*,*,#8414,.T.) ;
#11848 = ORIENTED_EDGE('',*,*,#8406,.T.) ;
#11849 = ORIENTED_EDGE('',*,*,#8419,.T.) ;
#11850 = ORIENTED_EDGE('',*,*,#8420,.F.) ;
#11851 = ORIENTED_EDGE('',*,*,#8416,.T.) ;
#11852 = ORIENTED_EDGE('',*,*,#8410,.T.) ;
#11853 = ORIENTED_EDGE('',*,*,#8421,.T.) ;
#11854 = ORIENTED_EDGE('',*,*,#8418,.T.) ;
#11855 = ORIENTED_EDGE('',*,*,#8422,.T.) ;
#11856 = ORIENTED_EDGE('',*,*,#8412,.T.) ;
#11857 = ORIENTED_EDGE('',*,*,#8415,.T.) ;
#11858 = ORIENTED_EDGE('',*,*,#8408,.T.) ;
#11859 = ORIENTED_EDGE('',*,*,#8417,.T.) ;
#11860 = ORIENTED_EDGE('',*,*,#8420,.T.) ;
#11861 = ORIENTED_EDGE('',*,*,#8423,.T.) ;
#11862 = ORIENTED_EDGE('',*,*,#8409,.F.) ;
#11863 = ORIENTED_EDGE('',*,*,#8423,.F.) ;
#11864 = ORIENTED_EDGE('',*,*,#8421,.F.) ;
#11865 = ORIENTED_EDGE('',*,*,#8413,.F.) ;
#11866 = ORIENTED_EDGE('',*,*,#8422,.F.) ;
#11867 = ORIENTED_EDGE('',*,*,#8419,.F.) ;
#11868 = ORIENTED_EDGE('',*,*,#8405,.T.) ;
#11869 = ORIENTED_EDGE('',*,*,#8424,.F.) ;
#11870 = ORIENTED_EDGE('',*,*,#8425,.T.) ;
#11871 = ORIENTED_EDGE('',*,*,#8426,.F.) ;
#11872 = ORIENTED_EDGE('',*,*,#8425,.F.) ;
#11873 = ORIENTED_EDGE('',*,*,#8424,.T.) ;
#11874 = ORIENTED_EDGE('',*,*,#8427,.F.) ;
#11875 = ORIENTED_EDGE('',*,*,#8428,.T.) ;
#11876 = ORIENTED_EDGE('',*,*,#8429,.F.) ;
#11877 = ORIENTED_EDGE('',*,*,#8430,.T.) ;
#11878 = ORIENTED_EDGE('',*,*,#8431,.F.) ;
#11879 = ORIENTED_EDGE('',*,*,#8432,.T.) ;
#11880 = ORIENTED_EDGE('',*,*,#8433,.F.) ;
#11881 = ORIENTED_EDGE('',*,*,#8434,.T.) ;
#11882 = ORIENTED_EDGE('',*,*,#8428,.F.) ;
#11883 = ORIENTED_EDGE('',*,*,#8435,.F.) ;
#11884 = ORIENTED_EDGE('',*,*,#8436,.F.) ;
#11885 = ORIENTED_EDGE('',*,*,#8432,.F.) ;
#11886 = ORIENTED_EDGE('',*,*,#8437,.F.) ;
#11887 = ORIENTED_EDGE('',*,*,#8438,.F.) ;
#11888 = ORIENTED_EDGE('',*,*,#8439,.F.) ;
#11889 = ORIENTED_EDGE('',*,*,#8435,.T.) ;
#11890 = ORIENTED_EDGE('',*,*,#8427,.T.) ;
#11891 = ORIENTED_EDGE('',*,*,#8440,.T.) ;
#11892 = ORIENTED_EDGE('',*,*,#8441,.F.) ;
#11893 = ORIENTED_EDGE('',*,*,#8437,.T.) ;
#11894 = ORIENTED_EDGE('',*,*,#8431,.T.) ;
#11895 = ORIENTED_EDGE('',*,*,#8442,.T.) ;
#11896 = ORIENTED_EDGE('',*,*,#8439,.T.) ;
#11897 = ORIENTED_EDGE('',*,*,#8443,.T.) ;
#11898 = ORIENTED_EDGE('',*,*,#8433,.T.) ;
#11899 = ORIENTED_EDGE('',*,*,#8436,.T.) ;
#11900 = ORIENTED_EDGE('',*,*,#8429,.T.) ;
#11901 = ORIENTED_EDGE('',*,*,#8438,.T.) ;
#11902 = ORIENTED_EDGE('',*,*,#8441,.T.) ;
#11903 = ORIENTED_EDGE('',*,*,#8444,.T.) ;
#11904 = ORIENTED_EDGE('',*,*,#8430,.F.) ;
#11905 = ORIENTED_EDGE('',*,*,#8444,.F.) ;
#11906 = ORIENTED_EDGE('',*,*,#8442,.F.) ;
#11907 = ORIENTED_EDGE('',*,*,#8434,.F.) ;
#11908 = ORIENTED_EDGE('',*,*,#8443,.F.) ;
#11909 = ORIENTED_EDGE('',*,*,#8440,.F.) ;
#11910 = ORIENTED_EDGE('',*,*,#8426,.T.) ;
#11911 = ORIENTED_EDGE('',*,*,#8445,.F.) ;
#11912 = ORIENTED_EDGE('',*,*,#8446,.T.) ;
#11913 = ORIENTED_EDGE('',*,*,#8447,.F.) ;
#11914 = ORIENTED_EDGE('',*,*,#8446,.F.) ;
#11915 = ORIENTED_EDGE('',*,*,#8445,.T.) ;
#11916 = ORIENTED_EDGE('',*,*,#8448,.F.) ;
#11917 = ORIENTED_EDGE('',*,*,#8449,.T.) ;
#11918 = ORIENTED_EDGE('',*,*,#8450,.F.) ;
#11919 = ORIENTED_EDGE('',*,*,#8451,.T.) ;
#11920 = ORIENTED_EDGE('',*,*,#8452,.F.) ;
#11921 = ORIENTED_EDGE('',*,*,#8453,.T.) ;
#11922 = ORIENTED_EDGE('',*,*,#8454,.F.) ;
#11923 = ORIENTED_EDGE('',*,*,#8455,.T.) ;
#11924 = ORIENTED_EDGE('',*,*,#8449,.F.) ;
#11925 = ORIENTED_EDGE('',*,*,#8456,.F.) ;
#11926 = ORIENTED_EDGE('',*,*,#8457,.F.) ;
#11927 = ORIENTED_EDGE('',*,*,#8453,.F.) ;
#11928 = ORIENTED_EDGE('',*,*,#8458,.F.) ;
#11929 = ORIENTED_EDGE('',*,*,#8459,.F.) ;
#11930 = ORIENTED_EDGE('',*,*,#8460,.F.) ;
#11931 = ORIENTED_EDGE('',*,*,#8456,.T.) ;
#11932 = ORIENTED_EDGE('',*,*,#8448,.T.) ;
#11933 = ORIENTED_EDGE('',*,*,#8461,.T.) ;
#11934 = ORIENTED_EDGE('',*,*,#8462,.F.) ;
#11935 = ORIENTED_EDGE('',*,*,#8458,.T.) ;
#11936 = ORIENTED_EDGE('',*,*,#8452,.T.) ;
#11937 = ORIENTED_EDGE('',*,*,#8463,.T.) ;
#11938 = ORIENTED_EDGE('',*,*,#8460,.T.) ;
#11939 = ORIENTED_EDGE('',*,*,#8464,.T.) ;
#11940 = ORIENTED_EDGE('',*,*,#8454,.T.) ;
#11941 = ORIENTED_EDGE('',*,*,#8457,.T.) ;
#11942 = ORIENTED_EDGE('',*,*,#8450,.T.) ;
#11943 = ORIENTED_EDGE('',*,*,#8459,.T.) ;
#11944 = ORIENTED_EDGE('',*,*,#8462,.T.) ;
#11945 = ORIENTED_EDGE('',*,*,#8465,.T.) ;
#11946 = ORIENTED_EDGE('',*,*,#8451,.F.) ;
#11947 = ORIENTED_EDGE('',*,*,#8465,.F.) ;
#11948 = ORIENTED_EDGE('',*,*,#8463,.F.) ;
#11949 = ORIENTED_EDGE('',*,*,#8455,.F.) ;
#11950 = ORIENTED_EDGE('',*,*,#8464,.F.) ;
#11951 = ORIENTED_EDGE('',*,*,#8461,.F.) ;
#11952 = ORIENTED_EDGE('',*,*,#8447,.T.) ;
#11953 = ORIENTED_EDGE('',*,*,#8466,.F.) ;
#11954 = ORIENTED_EDGE('',*,*,#8467,.T.) ;
#11955 = ORIENTED_EDGE('',*,*,#8468,.F.) ;
#11956 = ORIENTED_EDGE('',*,*,#8467,.F.) ;
#11957 = ORIENTED_EDGE('',*,*,#8469,.F.) ;
#11958 = ORIENTED_EDGE('',*,*,#8470,.T.) ;
#11959 = ORIENTED_EDGE('',*,*,#8471,.F.) ;
#11960 = ORIENTED_EDGE('',*,*,#8472,.T.) ;
#11961 = ORIENTED_EDGE('',*,*,#8473,.F.) ;
#11962 = ORIENTED_EDGE('',*,*,#8474,.T.) ;
#11963 = ORIENTED_EDGE('',*,*,#8475,.F.) ;
#11964 = ORIENTED_EDGE('',*,*,#8476,.T.) ;
#11965 = ORIENTED_EDGE('',*,*,#8470,.F.) ;
#11966 = ORIENTED_EDGE('',*,*,#8477,.F.) ;
#11967 = ORIENTED_EDGE('',*,*,#8478,.F.) ;
#11968 = ORIENTED_EDGE('',*,*,#8474,.F.) ;
#11969 = ORIENTED_EDGE('',*,*,#8479,.F.) ;
#11970 = ORIENTED_EDGE('',*,*,#8480,.F.) ;
#11971 = ORIENTED_EDGE('',*,*,#8466,.T.) ;
#11972 = ORIENTED_EDGE('',*,*,#8481,.F.) ;
#11973 = ORIENTED_EDGE('',*,*,#8477,.T.) ;
#11974 = ORIENTED_EDGE('',*,*,#8469,.T.) ;
#11975 = ORIENTED_EDGE('',*,*,#8482,.T.) ;
#11976 = ORIENTED_EDGE('',*,*,#8483,.F.) ;
#11977 = ORIENTED_EDGE('',*,*,#8479,.T.) ;
#11978 = ORIENTED_EDGE('',*,*,#8473,.T.) ;
#11979 = ORIENTED_EDGE('',*,*,#8484,.T.) ;
#11980 = ORIENTED_EDGE('',*,*,#8481,.T.) ;
#11981 = ORIENTED_EDGE('',*,*,#8485,.T.) ;
#11982 = ORIENTED_EDGE('',*,*,#8475,.T.) ;
#11983 = ORIENTED_EDGE('',*,*,#8478,.T.) ;
#11984 = ORIENTED_EDGE('',*,*,#8471,.T.) ;
#11985 = ORIENTED_EDGE('',*,*,#8480,.T.) ;
#11986 = ORIENTED_EDGE('',*,*,#8483,.T.) ;
#11987 = ORIENTED_EDGE('',*,*,#8486,.T.) ;
#11988 = ORIENTED_EDGE('',*,*,#8472,.F.) ;
#11989 = ORIENTED_EDGE('',*,*,#8486,.F.) ;
#11990 = ORIENTED_EDGE('',*,*,#8484,.F.) ;
#11991 = ORIENTED_EDGE('',*,*,#8476,.F.) ;
#11992 = ORIENTED_EDGE('',*,*,#8485,.F.) ;
#11993 = ORIENTED_EDGE('',*,*,#8482,.F.) ;
#11994 = ORIENTED_EDGE('',*,*,#8468,.T.) ;
#11995 = PLANE('',#13655) ;
#11996 = PLANE('',#13675) ;
#11997 = PLANE('',#13676) ;
#11998 = PLANE('',#13698) ;
#11999 = PLANE('',#13699) ;
#12000 = PLANE('',#13700) ;
#12001 = PLANE('',#13702) ;
#12002 = PLANE('',#13703) ;
#12003 = PLANE('',#13704) ;
#12004 = PLANE('',#13706) ;
#12005 = PLANE('',#13720) ;
#12006 = PLANE('',#13721) ;
#12007 = PLANE('',#13722) ;
#12008 = PLANE('',#13726) ;
#12009 = PLANE('',#13732) ;
#12010 = PLANE('',#13733) ;
#12011 = PLANE('',#13741) ;
#12012 = PLANE('',#13745) ;
#12013 = PLANE('',#13748) ;
#12014 = PLANE('',#13751) ;
#12015 = PLANE('',#13752) ;
#12016 = PLANE('',#13781) ;
#12017 = PLANE('',#13788) ;
#12018 = PLANE('',#13792) ;
#12019 = PLANE('',#13799) ;
#12020 = PLANE('',#13803) ;
#12021 = PLANE('',#13804) ;
#12022 = PLANE('',#13809) ;
#12023 = PLANE('',#13810) ;
#12024 = PLANE('',#13836) ;
#12025 = PLANE('',#13837) ;
#12026 = PLANE('',#13839) ;
#12027 = PLANE('',#13840) ;
#12028 = PLANE('',#13842) ;
#12029 = PLANE('',#13843) ;
#12030 = PLANE('',#13851) ;
#12031 = PLANE('',#13852) ;
#12032 = PLANE('',#13865) ;
#12033 = PLANE('',#13872) ;
#12034 = PLANE('',#13873) ;
#12035 = PLANE('',#13874) ;
#12036 = PLANE('',#13879) ;
#12037 = PLANE('',#13883) ;
#12038 = PLANE('',#13887) ;
#12039 = PLANE('',#13891) ;
#12040 = PLANE('',#13895) ;
#12041 = PLANE('',#13899) ;
#12042 = PLANE('',#13903) ;
#12043 = PLANE('',#13907) ;
#12044 = PLANE('',#13911) ;
#12045 = PLANE('',#13915) ;
#12046 = PLANE('',#13919) ;
#12047 = PLANE('',#13923) ;
#12048 = PLANE('',#13927) ;
#12049 = PLANE('',#13931) ;
#12050 = PLANE('',#13935) ;
#12051 = PLANE('',#13939) ;
#12052 = PLANE('',#13943) ;
#12053 = PLANE('',#13947) ;
#12054 = PLANE('',#13951) ;
#12055 = PLANE('',#13955) ;
#12056 = PLANE('',#13959) ;
#12057 = PLANE('',#13963) ;
#12058 = PLANE('',#13967) ;
#12059 = PLANE('',#13971) ;
#12060 = PLANE('',#14059) ;
#12061 = PLANE('',#14060) ;
#12062 = PLANE('',#14062) ;
#12063 = PLANE('',#14065) ;
#12064 = PLANE('',#14070) ;
#12065 = PLANE('',#14075) ;
#12066 = PLANE('',#14079) ;
#12067 = PLANE('',#14082) ;
#12068 = PLANE('',#14087) ;
#12069 = PLANE('',#14092) ;
#12070 = PLANE('',#14102) ;
#12071 = PLANE('',#14103) ;
#12072 = PLANE('',#14105) ;
#12073 = PLANE('',#14106) ;
#12074 = PLANE('',#14107) ;
#12075 = PLANE('',#14114) ;
#12076 = PLANE('',#14116) ;
#12077 = PLANE('',#14117) ;
#12078 = PLANE('',#14118) ;
#12079 = PLANE('',#14119) ;
#12080 = PLANE('',#14124) ;
#12081 = PLANE('',#14125) ;
#12082 = PLANE('',#14126) ;
#12083 = PLANE('',#14133) ;
#12084 = PLANE('',#14144) ;
#12085 = PLANE('',#14145) ;
#12086 = PLANE('',#14146) ;
#12087 = PLANE('',#14149) ;
#12088 = PLANE('',#14150) ;
#12089 = PLANE('',#14151) ;
#12090 = PLANE('',#14154) ;
#12091 = PLANE('',#14155) ;
#12092 = PLANE('',#14156) ;
#12093 = PLANE('',#14159) ;
#12094 = PLANE('',#14160) ;
#12095 = PLANE('',#14161) ;
#12096 = PLANE('',#14164) ;
#12097 = PLANE('',#14165) ;
#12098 = PLANE('',#14166) ;
#12099 = PLANE('',#14169) ;
#12100 = PLANE('',#14170) ;
#12101 = PLANE('',#14171) ;
#12102 = PLANE('',#14174) ;
#12103 = PLANE('',#14175) ;
#12104 = PLANE('',#14176) ;
#12105 = PLANE('',#14179) ;
#12106 = PLANE('',#14180) ;
#12107 = PLANE('',#14181) ;
#12108 = PLANE('',#14184) ;
#12109 = PLANE('',#14185) ;
#12110 = PLANE('',#14186) ;
#12111 = PLANE('',#14189) ;
#12112 = PLANE('',#14190) ;
#12113 = PLANE('',#14191) ;
#12114 = PLANE('',#14194) ;
#12115 = PLANE('',#14195) ;
#12116 = PLANE('',#14196) ;
#12117 = PLANE('',#14199) ;
#12118 = PLANE('',#14201) ;
#12119 = PLANE('',#14202) ;
#12120 = PLANE('',#14203) ;
#12121 = PLANE('',#14204) ;
#12122 = PLANE('',#14205) ;
#12123 = PLANE('',#14206) ;
#12124 = PLANE('',#14214) ;
#12125 = PLANE('',#14215) ;
#12126 = PLANE('',#14217) ;
#12127 = PLANE('',#14218) ;
#12128 = PLANE('',#14219) ;
#12129 = PLANE('',#14220) ;
#12130 = PLANE('',#14221) ;
#12131 = PLANE('',#14222) ;
#12132 = PLANE('',#14223) ;
#12133 = PLANE('',#14224) ;
#12134 = PLANE('',#14225) ;
#12135 = PLANE('',#14226) ;
#12136 = PLANE('',#14231) ;
#12137 = PLANE('',#14244) ;
#12138 = PLANE('',#14245) ;
#12139 = PLANE('',#14246) ;
#12140 = PLANE('',#14247) ;
#12141 = PLANE('',#14248) ;
#12142 = PLANE('',#14249) ;
#12143 = PLANE('',#14250) ;
#12144 = PLANE('',#14251) ;
#12145 = PLANE('',#14252) ;
#12146 = PLANE('',#14257) ;
#12147 = PLANE('',#14258) ;
#12148 = PLANE('',#14406) ;
#12149 = PLANE('',#14494) ;
#12150 = PLANE('',#14697) ;
#12151 = PLANE('',#14762) ;
#12152 = PLANE('',#14806) ;
#12153 = PLANE('',#14810) ;
#12154 = PLANE('',#14817) ;
#12155 = PLANE('',#14821) ;
#12156 = PLANE('',#14825) ;
#12157 = PLANE('',#14826) ;
#12158 = PLANE('',#14827) ;
#12159 = PLANE('',#14828) ;
#12160 = PLANE('',#14829) ;
#12161 = PLANE('',#14830) ;
#12162 = PLANE('',#14831) ;
#12163 = PLANE('',#14832) ;
#12164 = PLANE('',#14857) ;
#12165 = PLANE('',#14862) ;
#12166 = PLANE('',#14867) ;
#12167 = PLANE('',#14868) ;
#12168 = PLANE('',#14869) ;
#12169 = PLANE('',#14870) ;
#12170 = PLANE('',#14871) ;
#12171 = PLANE('',#14872) ;
#12172 = PLANE('',#14873) ;
#12173 = PLANE('',#14874) ;
#12174 = PLANE('',#14875) ;
#12175 = PLANE('',#14876) ;
#12176 = PLANE('',#14877) ;
#12177 = PLANE('',#14878) ;
#12178 = PLANE('',#14879) ;
#12179 = PLANE('',#14880) ;
#12180 = PLANE('',#14881) ;
#12181 = PLANE('',#14882) ;
#12182 = PLANE('',#14883) ;
#12183 = PLANE('',#14885) ;
#12184 = PLANE('',#14886) ;
#12185 = PLANE('',#14887) ;
#12186 = PLANE('',#14889) ;
#12187 = PLANE('',#14891) ;
#12188 = PLANE('',#14893) ;
#12189 = PLANE('',#14895) ;
#12190 = PLANE('',#14897) ;
#12191 = PLANE('',#14899) ;
#12192 = PLANE('',#14901) ;
#12193 = PLANE('',#14902) ;
#12194 = PLANE('',#14904) ;
#12195 = PLANE('',#14905) ;
#12196 = PLANE('',#14907) ;
#12197 = PLANE('',#14909) ;
#12198 = PLANE('',#14912) ;
#12199 = PLANE('',#14914) ;
#12200 = PLANE('',#14927) ;
#12201 = PLANE('',#14928) ;
#12202 = PLANE('',#14929) ;
#12203 = PLANE('',#14933) ;
#12204 = PLANE('',#14934) ;
#12205 = PLANE('',#14935) ;
#12206 = PLANE('',#14936) ;
#12207 = PLANE('',#14937) ;
#12208 = PLANE('',#14938) ;
#12209 = PLANE('',#14946) ;
#12210 = PLANE('',#14990) ;
#12211 = PLANE('',#14997) ;
#12212 = PLANE('',#14998) ;
#12213 = PLANE('',#15006) ;
#12214 = PLANE('',#15007) ;
#12215 = PLANE('',#15015) ;
#12216 = PLANE('',#15016) ;
#12217 = PLANE('',#15018) ;
#12218 = PLANE('',#15019) ;
#12219 = PLANE('',#15020) ;
#12220 = PLANE('',#15022) ;
#12221 = PLANE('',#15023) ;
#12222 = PLANE('',#15025) ;
#12223 = PLANE('',#15026) ;
#12224 = PLANE('',#15027) ;
#12225 = PLANE('',#15029) ;
#12226 = PLANE('',#15030) ;
#12227 = PLANE('',#15032) ;
#12228 = PLANE('',#15033) ;
#12229 = PLANE('',#15034) ;
#12230 = PLANE('',#15036) ;
#12231 = PLANE('',#15037) ;
#12232 = PLANE('',#15039) ;
#12233 = PLANE('',#15040) ;
#12234 = PLANE('',#15041) ;
#12235 = PLANE('',#15043) ;
#12236 = PLANE('',#15044) ;
#12237 = PLANE('',#15047) ;
#12238 = PLANE('',#15048) ;
#12239 = PLANE('',#15049) ;
#12240 = PLANE('',#15052) ;
#12241 = PLANE('',#15053) ;
#12242 = PLANE('',#15055) ;
#12243 = PLANE('',#15056) ;
#12244 = PLANE('',#15057) ;
#12245 = PLANE('',#15059) ;
#12246 = PLANE('',#15060) ;
#12247 = PLANE('',#15062) ;
#12248 = PLANE('',#15063) ;
#12249 = PLANE('',#15064) ;
#12250 = PLANE('',#15066) ;
#12251 = PLANE('',#15067) ;
#12252 = PLANE('',#15069) ;
#12253 = PLANE('',#15070) ;
#12254 = PLANE('',#15071) ;
#12255 = PLANE('',#15073) ;
#12256 = PLANE('',#15074) ;
#12257 = PLANE('',#15076) ;
#12258 = PLANE('',#15077) ;
#12259 = PLANE('',#15078) ;
#12260 = PLANE('',#15080) ;
#12261 = PLANE('',#15081) ;
#12262 = PLANE('',#15083) ;
#12263 = PLANE('',#15084) ;
#12264 = PLANE('',#15085) ;
#12265 = PLANE('',#15087) ;
#12266 = PLANE('',#15091) ;
#12267 = PLANE('',#15092) ;
#12268 = PLANE('',#15100) ;
#12269 = PLANE('',#15101) ;
#12270 = PLANE('',#15103) ;
#12271 = PLANE('',#15111) ;
#12272 = PLANE('',#15119) ;
#12273 = PLANE('',#15132) ;
#12274 = PLANE('',#15142) ;
#12275 = PLANE('',#15144) ;
#12276 = PLANE('',#15145) ;
#12277 = PLANE('',#15146) ;
#12278 = PLANE('',#15147) ;
#12279 = PLANE('',#15148) ;
#12280 = PLANE('',#15155) ;
#12281 = PLANE('',#15157) ;
#12282 = PLANE('',#15158) ;
#12283 = PLANE('',#15159) ;
#12284 = PLANE('',#15160) ;
#12285 = PLANE('',#15167) ;
#12286 = PLANE('',#15168) ;
#12287 = PLANE('',#15190) ;
#12288 = PLANE('',#15191) ;
#12289 = PLANE('',#15193) ;
#12290 = PLANE('',#15200) ;
#12291 = PLANE('',#15207) ;
#12292 = PLANE('',#15212) ;
#12293 = PLANE('',#15220) ;
#12294 = PLANE('',#15221) ;
#12295 = PLANE('',#15241) ;
#12296 = PLANE('',#15242) ;
#12297 = PLANE('',#15262) ;
#12298 = PLANE('',#15263) ;
#12299 = PLANE('',#15265) ;
#12300 = PLANE('',#15271) ;
#12301 = PLANE('',#15277) ;
#12302 = PLANE('',#15278) ;
#12303 = PLANE('',#15279) ;
#12304 = PLANE('',#15280) ;
#12305 = PLANE('',#15281) ;
#12306 = PLANE('',#15282) ;
#12307 = PLANE('',#15289) ;
#12308 = PLANE('',#15302) ;
#12309 = PLANE('',#15306) ;
#12310 = PLANE('',#15307) ;
#12311 = PLANE('',#15315) ;
#12312 = PLANE('',#15316) ;
#12313 = PLANE('',#15321) ;
#12314 = PLANE('',#15322) ;
#12315 = PLANE('',#15323) ;
#12316 = PLANE('',#15324) ;
#12317 = PLANE('',#15325) ;
#12318 = PLANE('',#15326) ;
#12319 = PLANE('',#15327) ;
#12320 = PLANE('',#15328) ;
#12321 = PLANE('',#15333) ;
#12322 = PLANE('',#15334) ;
#12323 = PLANE('',#15335) ;
#12324 = PLANE('',#15336) ;
#12325 = PLANE('',#15337) ;
#12326 = PLANE('',#15338) ;
#12327 = PLANE('',#15339) ;
#12328 = PLANE('',#15340) ;
#12329 = PLANE('',#15341) ;
#12330 = PLANE('',#15346) ;
#12331 = PLANE('',#15347) ;
#12332 = PLANE('',#15348) ;
#12333 = PLANE('',#15349) ;
#12334 = PLANE('',#15350) ;
#12335 = PLANE('',#15351) ;
#12336 = PLANE('',#15352) ;
#12337 = PLANE('',#15353) ;
#12338 = PLANE('',#15354) ;
#12339 = PLANE('',#15359) ;
#12340 = PLANE('',#15360) ;
#12341 = PLANE('',#15361) ;
#12342 = PLANE('',#15362) ;
#12343 = PLANE('',#15363) ;
#12344 = PLANE('',#15364) ;
#12345 = PLANE('',#15365) ;
#12346 = PLANE('',#15366) ;
#12347 = ADVANCED_FACE('',(#2952),#11995,.F.) ;
#12348 = ADVANCED_FACE('',(#2953),#2673,.F.) ;
#12349 = ADVANCED_FACE('',(#2954,#686),#2674,.F.) ;
#12350 = ADVANCED_FACE('',(#2955),#2675,.F.) ;
#12351 = ADVANCED_FACE('',(#2956),#11996,.F.) ;
#12352 = ADVANCED_FACE('',(#2957,#687),#11997,.F.) ;
#12353 = ADVANCED_FACE('',(#2958),#2676,.F.) ;
#12354 = ADVANCED_FACE('',(#2959),#2677,.F.) ;
#12355 = ADVANCED_FACE('',(#2960),#2678,.F.) ;
#12356 = ADVANCED_FACE('',(#2961),#2679,.F.) ;
#12357 = ADVANCED_FACE('',(#2962),#2680,.F.) ;
#12358 = ADVANCED_FACE('',(#2963),#2681,.F.) ;
#12359 = ADVANCED_FACE('',(#2964),#11998,.F.) ;
#12360 = ADVANCED_FACE('',(#2965),#11999,.F.) ;
#12361 = ADVANCED_FACE('',(#2966),#12000,.F.) ;
#12362 = ADVANCED_FACE('',(#2967),#12001,.T.) ;
#12363 = ADVANCED_FACE('',(#2968,#688,#689),#12002,.F.) ;
#12364 = ADVANCED_FACE('',(#2969),#12003,.F.) ;
#12365 = ADVANCED_FACE('',(#2970),#12004,.F.) ;
#12366 = ADVANCED_FACE('',(#2971,#690),#2682,.T.) ;
#12367 = ADVANCED_FACE('',(#2972),#2683,.F.) ;
#12368 = ADVANCED_FACE('',(#2973),#2684,.T.) ;
#12369 = ADVANCED_FACE('',(#2974),#2685,.T.) ;
#12370 = ADVANCED_FACE('',(#2975,#691),#12005,.T.) ;
#12371 = ADVANCED_FACE('',(#2976),#12006,.T.) ;
#12372 = ADVANCED_FACE('',(#2977),#12007,.F.) ;
#12373 = ADVANCED_FACE('',(#2978),#2686,.F.) ;
#12374 = ADVANCED_FACE('',(#2979),#12008,.T.) ;
#12375 = ADVANCED_FACE('',(#2980),#2687,.T.) ;
#12376 = ADVANCED_FACE('',(#2981,#692),#12009,.T.) ;
#12377 = ADVANCED_FACE('',(#2982,#693,#694,#695,#696,#697,#698,#699),#12010,
 .T.) ;
#12378 = ADVANCED_FACE('',(#2983),#2688,.F.) ;
#12379 = ADVANCED_FACE('',(#2984),#2689,.F.) ;
#12380 = ADVANCED_FACE('',(#2985,#700),#12011,.F.) ;
#12381 = ADVANCED_FACE('',(#2986),#2690,.F.) ;
#12382 = ADVANCED_FACE('',(#2987,#701),#12012,.F.) ;
#12383 = ADVANCED_FACE('',(#2988),#2691,.T.) ;
#12384 = ADVANCED_FACE('',(#2989,#702),#12013,.T.) ;
#12385 = ADVANCED_FACE('',(#2990),#2692,.T.) ;
#12386 = ADVANCED_FACE('',(#2991,#703),#12014,.T.) ;
#12387 = ADVANCED_FACE('',(#2992,#704,#705,#706,#707,#708,#709,#710),#12015,
 .T.) ;
#12388 = ADVANCED_FACE('',(#2993),#2693,.F.) ;
#12389 = ADVANCED_FACE('',(#2994),#2694,.F.) ;
#12390 = ADVANCED_FACE('',(#2995),#2695,.F.) ;
#12391 = ADVANCED_FACE('',(#2996),#2696,.F.) ;
#12392 = ADVANCED_FACE('',(#2997),#2697,.F.) ;
#12393 = ADVANCED_FACE('',(#2998),#2698,.F.) ;
#12394 = ADVANCED_FACE('',(#2999),#2699,.F.) ;
#12395 = ADVANCED_FACE('',(#3000),#2700,.F.) ;
#12396 = ADVANCED_FACE('',(#3001),#2701,.T.) ;
#12397 = ADVANCED_FACE('',(#3002,#711),#12016,.T.) ;
#12398 = ADVANCED_FACE('',(#3003),#2702,.F.) ;
#12399 = ADVANCED_FACE('',(#3004),#2703,.T.) ;
#12400 = ADVANCED_FACE('',(#3005,#712),#12017,.T.) ;
#12401 = ADVANCED_FACE('',(#3006),#2704,.F.) ;
#12402 = ADVANCED_FACE('',(#3007,#713),#12018,.F.) ;
#12403 = ADVANCED_FACE('',(#3008),#2705,.F.) ;
#12404 = ADVANCED_FACE('',(#3009),#2706,.F.) ;
#12405 = ADVANCED_FACE('',(#3010,#714,#715,#716,#717),#12019,.F.) ;
#12406 = ADVANCED_FACE('',(#3011),#2707,.T.) ;
#12407 = ADVANCED_FACE('',(#3012,#718,#719,#720,#721,#722,#723,#724),#12020,
 .T.) ;
#12408 = ADVANCED_FACE('',(#3013,#725,#726,#727,#728,#729,#730,#731,#732,
#733,#734),#12021,.T.) ;
#12409 = ADVANCED_FACE('',(#3014),#2708,.T.) ;
#12410 = ADVANCED_FACE('',(#3015),#12022,.T.) ;
#12411 = ADVANCED_FACE('',(#3016),#12023,.T.) ;
#12412 = ADVANCED_FACE('',(#3017),#2709,.F.) ;
#12413 = ADVANCED_FACE('',(#3018),#2710,.F.) ;
#12414 = ADVANCED_FACE('',(#3019),#2711,.F.) ;
#12415 = ADVANCED_FACE('',(#3020),#2712,.F.) ;
#12416 = ADVANCED_FACE('',(#3021),#2713,.F.) ;
#12417 = ADVANCED_FACE('',(#3022),#2714,.F.) ;
#12418 = ADVANCED_FACE('',(#3023),#2715,.F.) ;
#12419 = ADVANCED_FACE('',(#3024),#2716,.T.) ;
#12420 = ADVANCED_FACE('',(#3025,#735,#736,#737,#738,#739,#740,#741),#12024,
 .T.) ;
#12421 = ADVANCED_FACE('',(#3026,#742,#743,#744,#745,#746,#747,#748),#12025,
 .T.) ;
#12422 = ADVANCED_FACE('',(#3027),#12026,.F.) ;
#12423 = ADVANCED_FACE('',(#3028),#12027,.T.) ;
#12424 = ADVANCED_FACE('',(#3029),#12028,.T.) ;
#12425 = ADVANCED_FACE('',(#3030),#12029,.T.) ;
#12426 = ADVANCED_FACE('',(#3031),#2717,.T.) ;
#12427 = ADVANCED_FACE('',(#3032),#2718,.T.) ;
#12428 = ADVANCED_FACE('',(#3033,#749),#12030,.F.) ;
#12429 = ADVANCED_FACE('',(#3034,#750),#12031,.F.) ;
#12430 = ADVANCED_FACE('',(#3035),#2719,.T.) ;
#12431 = ADVANCED_FACE('',(#3036),#2720,.F.) ;
#12432 = ADVANCED_FACE('',(#3037),#2721,.F.) ;
#12433 = ADVANCED_FACE('',(#3038),#2722,.F.) ;
#12434 = ADVANCED_FACE('',(#3039,#751,#752,#753,#754),#12032,.T.) ;
#12435 = ADVANCED_FACE('',(#3040),#2723,.T.) ;
#12436 = ADVANCED_FACE('',(#3041),#2724,.T.) ;
#12437 = ADVANCED_FACE('',(#3042),#12033,.T.) ;
#12438 = ADVANCED_FACE('',(#3043),#12034,.T.) ;
#12439 = ADVANCED_FACE('',(#3044,#755,#756,#757,#758),#12035,.T.) ;
#12440 = ADVANCED_FACE('',(#3045),#2725,.F.) ;
#12441 = ADVANCED_FACE('',(#3046),#12036,.F.) ;
#12442 = ADVANCED_FACE('',(#3047),#2726,.F.) ;
#12443 = ADVANCED_FACE('',(#3048),#12037,.F.) ;
#12444 = ADVANCED_FACE('',(#3049),#2727,.F.) ;
#12445 = ADVANCED_FACE('',(#3050),#12038,.F.) ;
#12446 = ADVANCED_FACE('',(#3051),#2728,.F.) ;
#12447 = ADVANCED_FACE('',(#3052),#12039,.F.) ;
#12448 = ADVANCED_FACE('',(#3053),#2729,.F.) ;
#12449 = ADVANCED_FACE('',(#3054),#12040,.F.) ;
#12450 = ADVANCED_FACE('',(#3055),#2730,.F.) ;
#12451 = ADVANCED_FACE('',(#3056),#12041,.F.) ;
#12452 = ADVANCED_FACE('',(#3057),#2731,.F.) ;
#12453 = ADVANCED_FACE('',(#3058),#12042,.F.) ;
#12454 = ADVANCED_FACE('',(#3059),#2732,.F.) ;
#12455 = ADVANCED_FACE('',(#3060),#12043,.F.) ;
#12456 = ADVANCED_FACE('',(#3061),#2733,.F.) ;
#12457 = ADVANCED_FACE('',(#3062),#12044,.F.) ;
#12458 = ADVANCED_FACE('',(#3063),#2734,.F.) ;
#12459 = ADVANCED_FACE('',(#3064),#12045,.F.) ;
#12460 = ADVANCED_FACE('',(#3065),#2735,.F.) ;
#12461 = ADVANCED_FACE('',(#3066),#12046,.F.) ;
#12462 = ADVANCED_FACE('',(#3067),#2736,.F.) ;
#12463 = ADVANCED_FACE('',(#3068),#12047,.F.) ;
#12464 = ADVANCED_FACE('',(#3069),#2737,.F.) ;
#12465 = ADVANCED_FACE('',(#3070),#12048,.F.) ;
#12466 = ADVANCED_FACE('',(#3071),#2738,.F.) ;
#12467 = ADVANCED_FACE('',(#3072),#12049,.F.) ;
#12468 = ADVANCED_FACE('',(#3073),#2739,.F.) ;
#12469 = ADVANCED_FACE('',(#3074),#12050,.F.) ;
#12470 = ADVANCED_FACE('',(#3075),#2740,.F.) ;
#12471 = ADVANCED_FACE('',(#3076),#12051,.F.) ;
#12472 = ADVANCED_FACE('',(#3077),#2741,.F.) ;
#12473 = ADVANCED_FACE('',(#3078),#12052,.F.) ;
#12474 = ADVANCED_FACE('',(#3079),#2742,.F.) ;
#12475 = ADVANCED_FACE('',(#3080),#12053,.F.) ;
#12476 = ADVANCED_FACE('',(#3081),#2743,.F.) ;
#12477 = ADVANCED_FACE('',(#3082),#12054,.F.) ;
#12478 = ADVANCED_FACE('',(#3083),#2744,.F.) ;
#12479 = ADVANCED_FACE('',(#3084),#12055,.F.) ;
#12480 = ADVANCED_FACE('',(#3085),#2745,.F.) ;
#12481 = ADVANCED_FACE('',(#3086),#12056,.F.) ;
#12482 = ADVANCED_FACE('',(#3087),#2746,.F.) ;
#12483 = ADVANCED_FACE('',(#3088),#12057,.F.) ;
#12484 = ADVANCED_FACE('',(#3089),#2747,.F.) ;
#12485 = ADVANCED_FACE('',(#3090),#12058,.F.) ;
#12486 = ADVANCED_FACE('',(#3091),#2748,.F.) ;
#12487 = ADVANCED_FACE('',(#3092),#12059,.F.) ;
#12488 = ADVANCED_FACE('',(#3093),#2749,.F.) ;
#12489 = ADVANCED_FACE('',(#3094),#2750,.F.) ;
#12490 = ADVANCED_FACE('',(#3095),#2751,.F.) ;
#12491 = ADVANCED_FACE('',(#3096),#2752,.F.) ;
#12492 = ADVANCED_FACE('',(#3097),#2753,.F.) ;
#12493 = ADVANCED_FACE('',(#3098),#2754,.F.) ;
#12494 = ADVANCED_FACE('',(#3099),#2755,.F.) ;
#12495 = ADVANCED_FACE('',(#3100),#2756,.F.) ;
#12496 = ADVANCED_FACE('',(#3101),#2757,.F.) ;
#12497 = ADVANCED_FACE('',(#3102),#2758,.F.) ;
#12498 = ADVANCED_FACE('',(#3103),#2759,.F.) ;
#12499 = ADVANCED_FACE('',(#3104),#2760,.F.) ;
#12500 = ADVANCED_FACE('',(#3105),#2761,.F.) ;
#12501 = ADVANCED_FACE('',(#3106),#2762,.F.) ;
#12502 = ADVANCED_FACE('',(#3107),#2763,.F.) ;
#12503 = ADVANCED_FACE('',(#3108),#2764,.F.) ;
#12504 = ADVANCED_FACE('',(#3109),#2765,.F.) ;
#12505 = ADVANCED_FACE('',(#3110),#2766,.F.) ;
#12506 = ADVANCED_FACE('',(#3111),#2767,.F.) ;
#12507 = ADVANCED_FACE('',(#3112),#2768,.F.) ;
#12508 = ADVANCED_FACE('',(#3113),#2769,.F.) ;
#12509 = ADVANCED_FACE('',(#3114),#2770,.F.) ;
#12510 = ADVANCED_FACE('',(#3115),#2771,.F.) ;
#12511 = ADVANCED_FACE('',(#3116),#2772,.F.) ;
#12512 = ADVANCED_FACE('',(#3117),#2773,.F.) ;
#12513 = ADVANCED_FACE('',(#3118),#2774,.F.) ;
#12514 = ADVANCED_FACE('',(#3119),#2775,.F.) ;
#12515 = ADVANCED_FACE('',(#3120),#2776,.F.) ;
#12516 = ADVANCED_FACE('',(#3121),#2777,.T.) ;
#12517 = ADVANCED_FACE('',(#3122,#759,#760,#761,#762,#763,#764,#765,#766,
#767,#768,#769,#770,#771,#772,#773,#774,#775,#776,#777,#778,#779,#780,#781,
#782,#783,#784,#785,#786,#787,#788,#789,#790,#791,#792,#793,#794,#795,#796,
#797,#798,#799,#800,#801,#802,#803,#804,#805,#806,#807,#808,#809,#810),
#12060,.T.) ;
#12518 = ADVANCED_FACE('',(#3123,#811,#812,#813,#814,#815,#816,#817,#818,
#819,#820,#821,#822,#823,#824,#825,#826,#827,#828,#829,#830,#831,#832,#833,
#834,#835,#836,#837,#838),#12061,.T.) ;
#12519 = ADVANCED_FACE('',(#3124,#839),#12062,.T.) ;
#12520 = ADVANCED_FACE('',(#3125,#840),#12063,.T.) ;
#12521 = ADVANCED_FACE('',(#3126),#2778,.T.) ;
#12522 = ADVANCED_FACE('',(#3127),#2779,.F.) ;
#12523 = ADVANCED_FACE('',(#3128,#841),#12064,.T.) ;
#12524 = ADVANCED_FACE('',(#3129),#2780,.T.) ;
#12525 = ADVANCED_FACE('',(#3130,#842),#12065,.T.) ;
#12526 = ADVANCED_FACE('',(#3131),#2781,.F.) ;
#12527 = ADVANCED_FACE('',(#3132,#843),#12066,.T.) ;
#12528 = ADVANCED_FACE('',(#3133,#844),#12067,.T.) ;
#12529 = ADVANCED_FACE('',(#3134),#2782,.T.) ;
#12530 = ADVANCED_FACE('',(#3135),#2783,.F.) ;
#12531 = ADVANCED_FACE('',(#3136,#845),#12068,.T.) ;
#12532 = ADVANCED_FACE('',(#3137),#2784,.T.) ;
#12533 = ADVANCED_FACE('',(#3138,#846),#12069,.T.) ;
#12534 = ADVANCED_FACE('',(#3139),#2785,.F.) ;
#12535 = ADVANCED_FACE('',(#3140),#2786,.F.) ;
#12536 = ADVANCED_FACE('',(#3141),#2787,.T.) ;
#12537 = ADVANCED_FACE('',(#3142,#847),#12070,.T.) ;
#12538 = ADVANCED_FACE('',(#3143,#848),#12071,.T.) ;
#12539 = ADVANCED_FACE('',(#3144),#12072,.T.) ;
#12540 = ADVANCED_FACE('',(#3145),#12073,.T.) ;
#12541 = ADVANCED_FACE('',(#3146),#12074,.T.) ;
#12542 = ADVANCED_FACE('',(#3147),#2788,.F.) ;
#12543 = ADVANCED_FACE('',(#3148),#2789,.T.) ;
#12544 = ADVANCED_FACE('',(#3149),#12075,.T.) ;
#12545 = ADVANCED_FACE('',(#3150),#12076,.F.) ;
#12546 = ADVANCED_FACE('',(#3151),#12077,.T.) ;
#12547 = ADVANCED_FACE('',(#3152),#12078,.T.) ;
#12548 = ADVANCED_FACE('',(#3153,#849),#12079,.T.) ;
#12549 = ADVANCED_FACE('',(#3154),#2790,.F.) ;
#12550 = ADVANCED_FACE('',(#3155),#12080,.F.) ;
#12551 = ADVANCED_FACE('',(#3156),#12081,.T.) ;
#12552 = ADVANCED_FACE('',(#3157),#12082,.F.) ;
#12553 = ADVANCED_FACE('',(#3158),#2791,.T.) ;
#12554 = ADVANCED_FACE('',(#3159),#2792,.T.) ;
#12555 = ADVANCED_FACE('',(#3160,#850),#12083,.T.) ;
#12556 = ADVANCED_FACE('',(#3161),#12084,.T.) ;
#12557 = ADVANCED_FACE('',(#3162),#12085,.F.) ;
#12558 = ADVANCED_FACE('',(#3163),#12086,.F.) ;
#12559 = ADVANCED_FACE('',(#3164),#2793,.T.) ;
#12560 = ADVANCED_FACE('',(#3165),#12087,.F.) ;
#12561 = ADVANCED_FACE('',(#3166),#12088,.T.) ;
#12562 = ADVANCED_FACE('',(#3167),#12089,.F.) ;
#12563 = ADVANCED_FACE('',(#3168),#2794,.T.) ;
#12564 = ADVANCED_FACE('',(#3169),#12090,.T.) ;
#12565 = ADVANCED_FACE('',(#3170),#12091,.F.) ;
#12566 = ADVANCED_FACE('',(#3171),#12092,.F.) ;
#12567 = ADVANCED_FACE('',(#3172),#2795,.T.) ;
#12568 = ADVANCED_FACE('',(#3173),#12093,.F.) ;
#12569 = ADVANCED_FACE('',(#3174),#12094,.T.) ;
#12570 = ADVANCED_FACE('',(#3175),#12095,.F.) ;
#12571 = ADVANCED_FACE('',(#3176),#2796,.T.) ;
#12572 = ADVANCED_FACE('',(#3177),#12096,.T.) ;
#12573 = ADVANCED_FACE('',(#3178),#12097,.F.) ;
#12574 = ADVANCED_FACE('',(#3179),#12098,.F.) ;
#12575 = ADVANCED_FACE('',(#3180),#2797,.T.) ;
#12576 = ADVANCED_FACE('',(#3181),#12099,.F.) ;
#12577 = ADVANCED_FACE('',(#3182),#12100,.T.) ;
#12578 = ADVANCED_FACE('',(#3183),#12101,.F.) ;
#12579 = ADVANCED_FACE('',(#3184),#2798,.T.) ;
#12580 = ADVANCED_FACE('',(#3185),#12102,.T.) ;
#12581 = ADVANCED_FACE('',(#3186),#12103,.F.) ;
#12582 = ADVANCED_FACE('',(#3187),#12104,.F.) ;
#12583 = ADVANCED_FACE('',(#3188),#2799,.T.) ;
#12584 = ADVANCED_FACE('',(#3189),#12105,.F.) ;
#12585 = ADVANCED_FACE('',(#3190),#12106,.T.) ;
#12586 = ADVANCED_FACE('',(#3191),#12107,.F.) ;
#12587 = ADVANCED_FACE('',(#3192),#2800,.T.) ;
#12588 = ADVANCED_FACE('',(#3193),#12108,.T.) ;
#12589 = ADVANCED_FACE('',(#3194),#12109,.F.) ;
#12590 = ADVANCED_FACE('',(#3195),#12110,.F.) ;
#12591 = ADVANCED_FACE('',(#3196),#2801,.T.) ;
#12592 = ADVANCED_FACE('',(#3197),#12111,.F.) ;
#12593 = ADVANCED_FACE('',(#3198),#12112,.T.) ;
#12594 = ADVANCED_FACE('',(#3199),#12113,.F.) ;
#12595 = ADVANCED_FACE('',(#3200),#2802,.T.) ;
#12596 = ADVANCED_FACE('',(#3201),#12114,.T.) ;
#12597 = ADVANCED_FACE('',(#3202),#12115,.F.) ;
#12598 = ADVANCED_FACE('',(#3203),#12116,.F.) ;
#12599 = ADVANCED_FACE('',(#3204),#2803,.T.) ;
#12600 = ADVANCED_FACE('',(#3205,#851),#12117,.T.) ;
#12601 = ADVANCED_FACE('',(#3206),#12118,.T.) ;
#12602 = ADVANCED_FACE('',(#3207),#12119,.F.) ;
#12603 = ADVANCED_FACE('',(#3208),#12120,.F.) ;
#12604 = ADVANCED_FACE('',(#3209),#12121,.F.) ;
#12605 = ADVANCED_FACE('',(#3210),#12122,.F.) ;
#12606 = ADVANCED_FACE('',(#3211),#12123,.F.) ;
#12607 = ADVANCED_FACE('',(#3212),#2804,.F.) ;
#12608 = ADVANCED_FACE('',(#3213),#2805,.T.) ;
#12609 = ADVANCED_FACE('',(#3214,#852),#12124,.T.) ;
#12610 = ADVANCED_FACE('',(#3215,#853),#12125,.T.) ;
#12611 = ADVANCED_FACE('',(#3216),#12126,.T.) ;
#12612 = ADVANCED_FACE('',(#3217),#12127,.T.) ;
#12613 = ADVANCED_FACE('',(#3218),#12128,.T.) ;
#12614 = ADVANCED_FACE('',(#3219),#12129,.T.) ;
#12615 = ADVANCED_FACE('',(#3220),#12130,.F.) ;
#12616 = ADVANCED_FACE('',(#3221),#12131,.T.) ;
#12617 = ADVANCED_FACE('',(#3222),#12132,.F.) ;
#12618 = ADVANCED_FACE('',(#3223),#12133,.F.) ;
#12619 = ADVANCED_FACE('',(#3224),#12134,.F.) ;
#12620 = ADVANCED_FACE('',(#3225),#12135,.F.) ;
#12621 = ADVANCED_FACE('',(#3226),#2806,.T.) ;
#12622 = ADVANCED_FACE('',(#3227),#12136,.T.) ;
#12623 = ADVANCED_FACE('',(#3228),#2807,.F.) ;
#12624 = ADVANCED_FACE('',(#3229),#2808,.T.) ;
#12625 = ADVANCED_FACE('',(#3230),#2809,.T.) ;
#12626 = ADVANCED_FACE('',(#3231),#2810,.T.) ;
#12627 = ADVANCED_FACE('',(#3232),#12137,.T.) ;
#12628 = ADVANCED_FACE('',(#3233),#12138,.T.) ;
#12629 = ADVANCED_FACE('',(#3234),#12139,.F.) ;
#12630 = ADVANCED_FACE('',(#3235,#854),#12140,.F.) ;
#12631 = ADVANCED_FACE('',(#3236),#12141,.F.) ;
#12632 = ADVANCED_FACE('',(#3237),#12142,.F.) ;
#12633 = ADVANCED_FACE('',(#3238,#855,#856),#12143,.F.) ;
#12634 = ADVANCED_FACE('',(#3239),#12144,.F.) ;
#12635 = ADVANCED_FACE('',(#3240),#12145,.F.) ;
#12636 = ADVANCED_FACE('',(#3241),#2811,.T.) ;
#12637 = ADVANCED_FACE('',(#3242),#12146,.T.) ;
#12638 = ADVANCED_FACE('',(#3243),#12147,.T.) ;
#12639 = ADVANCED_FACE('',(#3244),#359,.T.) ;
#12640 = ADVANCED_FACE('',(#3245),#360,.T.) ;
#12641 = ADVANCED_FACE('',(#3246),#361,.T.) ;
#12642 = ADVANCED_FACE('',(#3247),#362,.T.) ;
#12643 = ADVANCED_FACE('',(#3248),#363,.T.) ;
#12644 = ADVANCED_FACE('',(#3249),#364,.T.) ;
#12645 = ADVANCED_FACE('',(#3250),#365,.T.) ;
#12646 = ADVANCED_FACE('',(#3251),#366,.T.) ;
#12647 = ADVANCED_FACE('',(#3252),#367,.T.) ;
#12648 = ADVANCED_FACE('',(#3253),#368,.T.) ;
#12649 = ADVANCED_FACE('',(#3254),#369,.T.) ;
#12650 = ADVANCED_FACE('',(#3255),#370,.T.) ;
#12651 = ADVANCED_FACE('',(#3256),#371,.T.) ;
#12652 = ADVANCED_FACE('',(#3257),#372,.T.) ;
#12653 = ADVANCED_FACE('',(#3258),#373,.T.) ;
#12654 = ADVANCED_FACE('',(#3259),#374,.T.) ;
#12655 = ADVANCED_FACE('',(#3260),#375,.T.) ;
#12656 = ADVANCED_FACE('',(#3261),#376,.T.) ;
#12657 = ADVANCED_FACE('',(#3262),#377,.T.) ;
#12658 = ADVANCED_FACE('',(#3263),#378,.T.) ;
#12659 = ADVANCED_FACE('',(#3264),#379,.T.) ;
#12660 = ADVANCED_FACE('',(#3265),#380,.T.) ;
#12661 = ADVANCED_FACE('',(#3266),#381,.T.) ;
#12662 = ADVANCED_FACE('',(#3267),#382,.T.) ;
#12663 = ADVANCED_FACE('',(#3268),#383,.T.) ;
#12664 = ADVANCED_FACE('',(#3269),#384,.T.) ;
#12665 = ADVANCED_FACE('',(#3270),#385,.T.) ;
#12666 = ADVANCED_FACE('',(#3271),#386,.T.) ;
#12667 = ADVANCED_FACE('',(#3272),#387,.T.) ;
#12668 = ADVANCED_FACE('',(#3273),#388,.T.) ;
#12669 = ADVANCED_FACE('',(#3274),#389,.T.) ;
#12670 = ADVANCED_FACE('',(#3275),#2812,.T.) ;
#12671 = ADVANCED_FACE('',(#3276),#12148,.T.) ;
#12672 = ADVANCED_FACE('',(#3277),#2813,.T.) ;
#12673 = ADVANCED_FACE('',(#3278),#2814,.T.) ;
#12674 = ADVANCED_FACE('',(#3279),#2815,.T.) ;
#12675 = ADVANCED_FACE('',(#3280),#2816,.T.) ;
#12676 = ADVANCED_FACE('',(#3281),#2817,.T.) ;
#12677 = ADVANCED_FACE('',(#3282),#2818,.T.) ;
#12678 = ADVANCED_FACE('',(#3283),#2819,.T.) ;
#12679 = ADVANCED_FACE('',(#3284),#2820,.T.) ;
#12680 = ADVANCED_FACE('',(#3285),#2821,.T.) ;
#12681 = ADVANCED_FACE('',(#3286),#2822,.T.) ;
#12682 = ADVANCED_FACE('',(#3287),#2823,.T.) ;
#12683 = ADVANCED_FACE('',(#3288),#2824,.T.) ;
#12684 = ADVANCED_FACE('',(#3289),#2825,.T.) ;
#12685 = ADVANCED_FACE('',(#3290),#2826,.T.) ;
#12686 = ADVANCED_FACE('',(#3291),#2827,.T.) ;
#12687 = ADVANCED_FACE('',(#3292),#2828,.T.) ;
#12688 = ADVANCED_FACE('',(#3293),#2829,.T.) ;
#12689 = ADVANCED_FACE('',(#3294),#2830,.T.) ;
#12690 = ADVANCED_FACE('',(#3295),#2831,.T.) ;
#12691 = ADVANCED_FACE('',(#3296),#2832,.T.) ;
#12692 = ADVANCED_FACE('',(#3297),#2833,.T.) ;
#12693 = ADVANCED_FACE('',(#3298),#2834,.T.) ;
#12694 = ADVANCED_FACE('',(#3299),#2835,.T.) ;
#12695 = ADVANCED_FACE('',(#3300),#2836,.T.) ;
#12696 = ADVANCED_FACE('',(#3301),#2837,.T.) ;
#12697 = ADVANCED_FACE('',(#3302),#2838,.T.) ;
#12698 = ADVANCED_FACE('',(#3303),#2839,.T.) ;
#12699 = ADVANCED_FACE('',(#3304),#2840,.T.) ;
#12700 = ADVANCED_FACE('',(#3305),#2841,.T.) ;
#12701 = ADVANCED_FACE('',(#3306),#2842,.T.) ;
#12702 = ADVANCED_FACE('',(#3307),#2843,.T.) ;
#12703 = ADVANCED_FACE('',(#3308),#12149,.T.) ;
#12704 = ADVANCED_FACE('',(#3309),#390,.F.) ;
#12705 = ADVANCED_FACE('',(#3310),#391,.T.) ;
#12706 = ADVANCED_FACE('',(#3311),#392,.F.) ;
#12707 = ADVANCED_FACE('',(#3312),#393,.F.) ;
#12708 = ADVANCED_FACE('',(#3313),#394,.F.) ;
#12709 = ADVANCED_FACE('',(#3314),#2844,.F.) ;
#12710 = ADVANCED_FACE('',(#3315),#395,.T.) ;
#12711 = ADVANCED_FACE('',(#3316),#396,.T.) ;
#12712 = ADVANCED_FACE('',(#3317),#397,.F.) ;
#12713 = ADVANCED_FACE('',(#3318),#398,.T.) ;
#12714 = ADVANCED_FACE('',(#3319),#2845,.T.) ;
#12715 = ADVANCED_FACE('',(#3320),#399,.F.) ;
#12716 = ADVANCED_FACE('',(#3321),#400,.T.) ;
#12717 = ADVANCED_FACE('',(#3322),#401,.T.) ;
#12718 = ADVANCED_FACE('',(#3323),#402,.F.) ;
#12719 = ADVANCED_FACE('',(#3324),#403,.F.) ;
#12720 = ADVANCED_FACE('',(#3325),#404,.T.) ;
#12721 = ADVANCED_FACE('',(#3326),#405,.F.) ;
#12722 = ADVANCED_FACE('',(#3327),#406,.T.) ;
#12723 = ADVANCED_FACE('',(#3328),#407,.F.) ;
#12724 = ADVANCED_FACE('',(#3329),#408,.T.) ;
#12725 = ADVANCED_FACE('',(#3330),#409,.T.) ;
#12726 = ADVANCED_FACE('',(#3331),#410,.F.) ;
#12727 = ADVANCED_FACE('',(#3332),#411,.F.) ;
#12728 = ADVANCED_FACE('',(#3333),#412,.T.) ;
#12729 = ADVANCED_FACE('',(#3334),#413,.F.) ;
#12730 = ADVANCED_FACE('',(#3335),#414,.T.) ;
#12731 = ADVANCED_FACE('',(#3336),#415,.F.) ;
#12732 = ADVANCED_FACE('',(#3337),#416,.T.) ;
#12733 = ADVANCED_FACE('',(#3338),#417,.T.) ;
#12734 = ADVANCED_FACE('',(#3339),#418,.F.) ;
#12735 = ADVANCED_FACE('',(#3340),#419,.F.) ;
#12736 = ADVANCED_FACE('',(#3341),#420,.T.) ;
#12737 = ADVANCED_FACE('',(#3342),#421,.F.) ;
#12738 = ADVANCED_FACE('',(#3343),#422,.T.) ;
#12739 = ADVANCED_FACE('',(#3344),#423,.F.) ;
#12740 = ADVANCED_FACE('',(#3345),#424,.T.) ;
#12741 = ADVANCED_FACE('',(#3346),#425,.T.) ;
#12742 = ADVANCED_FACE('',(#3347),#426,.F.) ;
#12743 = ADVANCED_FACE('',(#3348),#427,.F.) ;
#12744 = ADVANCED_FACE('',(#3349),#428,.T.) ;
#12745 = ADVANCED_FACE('',(#3350),#429,.F.) ;
#12746 = ADVANCED_FACE('',(#3351),#430,.T.) ;
#12747 = ADVANCED_FACE('',(#3352,#857),#431,.F.) ;
#12748 = ADVANCED_FACE('',(#3353),#432,.T.) ;
#12749 = ADVANCED_FACE('',(#3354),#433,.T.) ;
#12750 = ADVANCED_FACE('',(#3355),#434,.F.) ;
#12751 = ADVANCED_FACE('',(#3356),#435,.F.) ;
#12752 = ADVANCED_FACE('',(#3357),#436,.T.) ;
#12753 = ADVANCED_FACE('',(#3358,#858),#437,.F.) ;
#12754 = ADVANCED_FACE('',(#3359),#438,.T.) ;
#12755 = ADVANCED_FACE('',(#3360,#859),#439,.F.) ;
#12756 = ADVANCED_FACE('',(#3361),#440,.T.) ;
#12757 = ADVANCED_FACE('',(#3362),#441,.T.) ;
#12758 = ADVANCED_FACE('',(#3363),#442,.F.) ;
#12759 = ADVANCED_FACE('',(#3364),#443,.F.) ;
#12760 = ADVANCED_FACE('',(#3365),#444,.T.) ;
#12761 = ADVANCED_FACE('',(#3366),#2846,.F.) ;
#12762 = ADVANCED_FACE('',(#3367),#445,.F.) ;
#12763 = ADVANCED_FACE('',(#3368),#446,.F.) ;
#12764 = ADVANCED_FACE('',(#3369),#447,.F.) ;
#12765 = ADVANCED_FACE('',(#3370),#448,.T.) ;
#12766 = ADVANCED_FACE('',(#3371),#449,.F.) ;
#12767 = ADVANCED_FACE('',(#3372),#450,.T.) ;
#12768 = ADVANCED_FACE('',(#3373,#860),#451,.F.) ;
#12769 = ADVANCED_FACE('',(#3374),#2847,.T.) ;
#12770 = ADVANCED_FACE('',(#3375),#452,.T.) ;
#12771 = ADVANCED_FACE('',(#3376),#453,.T.) ;
#12772 = ADVANCED_FACE('',(#3377),#454,.T.) ;
#12773 = ADVANCED_FACE('',(#3378),#455,.T.) ;
#12774 = ADVANCED_FACE('',(#3379),#456,.T.) ;
#12775 = ADVANCED_FACE('',(#3380),#457,.T.) ;
#12776 = ADVANCED_FACE('',(#3381),#458,.T.) ;
#12777 = ADVANCED_FACE('',(#3382),#459,.T.) ;
#12778 = ADVANCED_FACE('',(#3383),#460,.T.) ;
#12779 = ADVANCED_FACE('',(#3384),#2848,.F.) ;
#12780 = ADVANCED_FACE('',(#3385),#2849,.T.) ;
#12781 = ADVANCED_FACE('',(#3386,#861),#12150,.T.) ;
#12782 = ADVANCED_FACE('',(#3387),#2850,.T.) ;
#12783 = ADVANCED_FACE('',(#3388),#2851,.T.) ;
#12784 = ADVANCED_FACE('',(#3389),#2852,.T.) ;
#12785 = ADVANCED_FACE('',(#3390),#2853,.T.) ;
#12786 = ADVANCED_FACE('',(#3391),#2854,.T.) ;
#12787 = ADVANCED_FACE('',(#3392),#2855,.T.) ;
#12788 = ADVANCED_FACE('',(#3393),#2856,.T.) ;
#12789 = ADVANCED_FACE('',(#3394),#2857,.T.) ;
#12790 = ADVANCED_FACE('',(#3395),#2858,.T.) ;
#12791 = ADVANCED_FACE('',(#3396),#2859,.T.) ;
#12792 = ADVANCED_FACE('',(#3397),#2860,.T.) ;
#12793 = ADVANCED_FACE('',(#3398),#2861,.T.) ;
#12794 = ADVANCED_FACE('',(#3399),#2862,.T.) ;
#12795 = ADVANCED_FACE('',(#3400),#2863,.T.) ;
#12796 = ADVANCED_FACE('',(#3401),#2864,.T.) ;
#12797 = ADVANCED_FACE('',(#3402),#2865,.T.) ;
#12798 = ADVANCED_FACE('',(#3403),#2866,.T.) ;
#12799 = ADVANCED_FACE('',(#3404,#862),#12151,.T.) ;
#12800 = ADVANCED_FACE('',(#3405),#461,.T.) ;
#12801 = ADVANCED_FACE('',(#3406),#462,.T.) ;
#12802 = ADVANCED_FACE('',(#3407),#463,.T.) ;
#12803 = ADVANCED_FACE('',(#3408),#464,.T.) ;
#12804 = ADVANCED_FACE('',(#3409),#465,.T.) ;
#12805 = ADVANCED_FACE('',(#3410),#466,.T.) ;
#12806 = ADVANCED_FACE('',(#3411),#467,.T.) ;
#12807 = ADVANCED_FACE('',(#3412),#2867,.F.) ;
#12808 = ADVANCED_FACE('',(#3413),#468,.T.) ;
#12809 = ADVANCED_FACE('',(#3414),#469,.T.) ;
#12810 = ADVANCED_FACE('',(#3415),#470,.F.) ;
#12811 = ADVANCED_FACE('',(#3416),#471,.F.) ;
#12812 = ADVANCED_FACE('',(#3417),#472,.F.) ;
#12813 = ADVANCED_FACE('',(#3418),#473,.F.) ;
#12814 = ADVANCED_FACE('',(#3419),#474,.F.) ;
#12815 = ADVANCED_FACE('',(#3420),#475,.F.) ;
#12816 = ADVANCED_FACE('',(#3421),#476,.F.) ;
#12817 = ADVANCED_FACE('',(#3422),#477,.F.) ;
#12818 = ADVANCED_FACE('',(#3423),#478,.F.) ;
#12819 = ADVANCED_FACE('',(#3424),#479,.F.) ;
#12820 = ADVANCED_FACE('',(#3425),#480,.F.) ;
#12821 = ADVANCED_FACE('',(#3426),#481,.F.) ;
#12822 = ADVANCED_FACE('',(#3427),#2868,.F.) ;
#12823 = ADVANCED_FACE('',(#3428),#12152,.T.) ;
#12824 = ADVANCED_FACE('',(#3429),#2869,.F.) ;
#12825 = ADVANCED_FACE('',(#3430),#12153,.T.) ;
#12826 = ADVANCED_FACE('',(#3431),#2870,.F.) ;
#12827 = ADVANCED_FACE('',(#3432),#2871,.F.) ;
#12828 = ADVANCED_FACE('',(#3433),#12154,.T.) ;
#12829 = ADVANCED_FACE('',(#3434),#2872,.F.) ;
#12830 = ADVANCED_FACE('',(#3435),#12155,.T.) ;
#12831 = ADVANCED_FACE('',(#3436),#2873,.F.) ;
#12832 = ADVANCED_FACE('',(#3437,#863,#864),#12156,.F.) ;
#12833 = ADVANCED_FACE('',(#3438),#12157,.F.) ;
#12834 = ADVANCED_FACE('',(#3439,#865,#866),#12158,.F.) ;
#12835 = ADVANCED_FACE('',(#3440),#12159,.F.) ;
#12836 = ADVANCED_FACE('',(#3441,#867,#868),#12160,.T.) ;
#12837 = ADVANCED_FACE('',(#3442),#12161,.F.) ;
#12838 = ADVANCED_FACE('',(#3443,#869,#870),#12162,.F.) ;
#12839 = ADVANCED_FACE('',(#3444),#12163,.F.) ;
#12840 = ADVANCED_FACE('',(#3445),#13,.T.) ;
#12841 = ADVANCED_FACE('',(#3446),#14,.T.) ;
#12842 = ADVANCED_FACE('',(#3447),#15,.T.) ;
#12843 = ADVANCED_FACE('',(#3448),#16,.T.) ;
#12844 = ADVANCED_FACE('',(#3449,#871),#12164,.F.) ;
#12845 = ADVANCED_FACE('',(#3450,#872),#12165,.T.) ;
#12846 = ADVANCED_FACE('',(#3451),#17,.F.) ;
#12847 = ADVANCED_FACE('',(#3452),#18,.F.) ;
#12848 = ADVANCED_FACE('',(#3453),#19,.F.) ;
#12849 = ADVANCED_FACE('',(#3454),#20,.F.) ;
#12850 = ADVANCED_FACE('',(#3455),#2874,.T.) ;
#12851 = ADVANCED_FACE('',(#3456),#12166,.T.) ;
#12852 = ADVANCED_FACE('',(#3457),#12167,.T.) ;
#12853 = ADVANCED_FACE('',(#3458),#12168,.T.) ;
#12854 = ADVANCED_FACE('',(#3459),#12169,.F.) ;
#12855 = ADVANCED_FACE('',(#3460),#12170,.T.) ;
#12856 = ADVANCED_FACE('',(#3461),#12171,.T.) ;
#12857 = ADVANCED_FACE('',(#3462,#873),#12172,.F.) ;
#12858 = ADVANCED_FACE('',(#3463),#12173,.F.) ;
#12859 = ADVANCED_FACE('',(#3464),#12174,.F.) ;
#12860 = ADVANCED_FACE('',(#3465),#12175,.F.) ;
#12861 = ADVANCED_FACE('',(#3466),#12176,.F.) ;
#12862 = ADVANCED_FACE('',(#3467,#874),#12177,.T.) ;
#12863 = ADVANCED_FACE('',(#3468,#875),#12178,.F.) ;
#12864 = ADVANCED_FACE('',(#3469),#12179,.F.) ;
#12865 = ADVANCED_FACE('',(#3470),#12180,.F.) ;
#12866 = ADVANCED_FACE('',(#3471),#12181,.F.) ;
#12867 = ADVANCED_FACE('',(#3472),#12182,.F.) ;
#12868 = ADVANCED_FACE('',(#3473),#12183,.T.) ;
#12869 = ADVANCED_FACE('',(#3474),#12184,.T.) ;
#12870 = ADVANCED_FACE('',(#3475),#12185,.T.) ;
#12871 = ADVANCED_FACE('',(#3476),#12186,.T.) ;
#12872 = ADVANCED_FACE('',(#3477),#12187,.T.) ;
#12873 = ADVANCED_FACE('',(#3478),#12188,.F.) ;
#12874 = ADVANCED_FACE('',(#3479),#12189,.F.) ;
#12875 = ADVANCED_FACE('',(#3480),#12190,.F.) ;
#12876 = ADVANCED_FACE('',(#3481),#12191,.F.) ;
#12877 = ADVANCED_FACE('',(#3482),#12192,.T.) ;
#12878 = ADVANCED_FACE('',(#3483),#12193,.T.) ;
#12879 = ADVANCED_FACE('',(#3484),#12194,.T.) ;
#12880 = ADVANCED_FACE('',(#3485),#12195,.F.) ;
#12881 = ADVANCED_FACE('',(#3486),#12196,.F.) ;
#12882 = ADVANCED_FACE('',(#3487),#12197,.F.) ;
#12883 = ADVANCED_FACE('',(#3488),#12198,.F.) ;
#12884 = ADVANCED_FACE('',(#3489),#12199,.F.) ;
#12885 = ADVANCED_FACE('',(#3490),#2875,.F.) ;
#12886 = ADVANCED_FACE('',(#3491),#2876,.F.) ;
#12887 = ADVANCED_FACE('',(#3492),#2877,.F.) ;
#12888 = ADVANCED_FACE('',(#3493,#876,#877),#2878,.F.) ;
#12889 = ADVANCED_FACE('',(#3494,#878),#12200,.F.) ;
#12890 = ADVANCED_FACE('',(#3495,#879),#12201,.F.) ;
#12891 = ADVANCED_FACE('',(#3496),#12202,.F.) ;
#12892 = ADVANCED_FACE('',(#3497),#2879,.F.) ;
#12893 = ADVANCED_FACE('',(#3498,#880),#12203,.T.) ;
#12894 = ADVANCED_FACE('',(#3499,#881),#12204,.F.) ;
#12895 = ADVANCED_FACE('',(#3500,#882),#12205,.F.) ;
#12896 = ADVANCED_FACE('',(#3501),#12206,.F.) ;
#12897 = ADVANCED_FACE('',(#3502,#883),#12207,.F.) ;
#12898 = ADVANCED_FACE('',(#3503),#12208,.F.) ;
#12899 = ADVANCED_FACE('',(#3504),#2880,.F.) ;
#12900 = ADVANCED_FACE('',(#3505),#2881,.F.) ;
#12901 = ADVANCED_FACE('',(#3506,#884),#12209,.T.) ;
#12902 = ADVANCED_FACE('',(#3507),#2882,.T.) ;
#12903 = ADVANCED_FACE('',(#3508),#2883,.F.) ;
#12904 = ADVANCED_FACE('',(#3509),#2884,.T.) ;
#12905 = ADVANCED_FACE('',(#3510),#2885,.F.) ;
#12906 = ADVANCED_FACE('',(#3511),#2886,.T.) ;
#12907 = ADVANCED_FACE('',(#3512),#2887,.F.) ;
#12908 = ADVANCED_FACE('',(#3513),#2888,.T.) ;
#12909 = ADVANCED_FACE('',(#3514),#2889,.F.) ;
#12910 = ADVANCED_FACE('',(#3515),#2890,.T.) ;
#12911 = ADVANCED_FACE('',(#3516),#2891,.F.) ;
#12912 = ADVANCED_FACE('',(#3517),#2892,.T.) ;
#12913 = ADVANCED_FACE('',(#3518),#2893,.F.) ;
#12914 = ADVANCED_FACE('',(#3519),#2894,.T.) ;
#12915 = ADVANCED_FACE('',(#3520),#2895,.F.) ;
#12916 = ADVANCED_FACE('',(#3521,#885),#12210,.T.) ;
#12917 = ADVANCED_FACE('',(#3522),#2896,.T.) ;
#12918 = ADVANCED_FACE('',(#3523),#2897,.T.) ;
#12919 = ADVANCED_FACE('',(#3524),#12211,.T.) ;
#12920 = ADVANCED_FACE('',(#3525),#12212,.T.) ;
#12921 = ADVANCED_FACE('',(#3526),#2898,.F.) ;
#12922 = ADVANCED_FACE('',(#3527),#2899,.T.) ;
#12923 = ADVANCED_FACE('',(#3528,#886),#12213,.T.) ;
#12924 = ADVANCED_FACE('',(#3529,#887),#12214,.T.) ;
#12925 = ADVANCED_FACE('',(#3530),#2900,.F.) ;
#12926 = ADVANCED_FACE('',(#3531),#2901,.T.) ;
#12927 = ADVANCED_FACE('',(#3532,#888),#12215,.T.) ;
#12928 = ADVANCED_FACE('',(#3533),#12216,.F.) ;
#12929 = ADVANCED_FACE('',(#3534),#12217,.F.) ;
#12930 = ADVANCED_FACE('',(#3535),#12218,.T.) ;
#12931 = ADVANCED_FACE('',(#3536),#12219,.F.) ;
#12932 = ADVANCED_FACE('',(#3537),#12220,.F.) ;
#12933 = ADVANCED_FACE('',(#3538),#12221,.F.) ;
#12934 = ADVANCED_FACE('',(#3539),#12222,.F.) ;
#12935 = ADVANCED_FACE('',(#3540),#12223,.T.) ;
#12936 = ADVANCED_FACE('',(#3541),#12224,.F.) ;
#12937 = ADVANCED_FACE('',(#3542),#12225,.F.) ;
#12938 = ADVANCED_FACE('',(#3543),#12226,.F.) ;
#12939 = ADVANCED_FACE('',(#3544),#12227,.F.) ;
#12940 = ADVANCED_FACE('',(#3545),#12228,.T.) ;
#12941 = ADVANCED_FACE('',(#3546),#12229,.F.) ;
#12942 = ADVANCED_FACE('',(#3547),#12230,.F.) ;
#12943 = ADVANCED_FACE('',(#3548),#12231,.F.) ;
#12944 = ADVANCED_FACE('',(#3549),#12232,.F.) ;
#12945 = ADVANCED_FACE('',(#3550),#12233,.T.) ;
#12946 = ADVANCED_FACE('',(#3551),#12234,.F.) ;
#12947 = ADVANCED_FACE('',(#3552),#12235,.F.) ;
#12948 = ADVANCED_FACE('',(#3553),#12236,.F.) ;
#12949 = ADVANCED_FACE('',(#3554),#12237,.F.) ;
#12950 = ADVANCED_FACE('',(#3555),#12238,.T.) ;
#12951 = ADVANCED_FACE('',(#3556),#12239,.F.) ;
#12952 = ADVANCED_FACE('',(#3557),#12240,.F.) ;
#12953 = ADVANCED_FACE('',(#3558),#12241,.F.) ;
#12954 = ADVANCED_FACE('',(#3559),#12242,.F.) ;
#12955 = ADVANCED_FACE('',(#3560),#12243,.T.) ;
#12956 = ADVANCED_FACE('',(#3561),#12244,.F.) ;
#12957 = ADVANCED_FACE('',(#3562),#12245,.F.) ;
#12958 = ADVANCED_FACE('',(#3563),#12246,.F.) ;
#12959 = ADVANCED_FACE('',(#3564),#12247,.F.) ;
#12960 = ADVANCED_FACE('',(#3565),#12248,.T.) ;
#12961 = ADVANCED_FACE('',(#3566),#12249,.F.) ;
#12962 = ADVANCED_FACE('',(#3567),#12250,.F.) ;
#12963 = ADVANCED_FACE('',(#3568),#12251,.F.) ;
#12964 = ADVANCED_FACE('',(#3569),#12252,.F.) ;
#12965 = ADVANCED_FACE('',(#3570),#12253,.T.) ;
#12966 = ADVANCED_FACE('',(#3571),#12254,.F.) ;
#12967 = ADVANCED_FACE('',(#3572),#12255,.F.) ;
#12968 = ADVANCED_FACE('',(#3573),#12256,.F.) ;
#12969 = ADVANCED_FACE('',(#3574),#12257,.F.) ;
#12970 = ADVANCED_FACE('',(#3575),#12258,.T.) ;
#12971 = ADVANCED_FACE('',(#3576),#12259,.F.) ;
#12972 = ADVANCED_FACE('',(#3577),#12260,.F.) ;
#12973 = ADVANCED_FACE('',(#3578),#12261,.F.) ;
#12974 = ADVANCED_FACE('',(#3579),#12262,.F.) ;
#12975 = ADVANCED_FACE('',(#3580),#12263,.T.) ;
#12976 = ADVANCED_FACE('',(#3581),#12264,.F.) ;
#12977 = ADVANCED_FACE('',(#3582),#12265,.F.) ;
#12978 = ADVANCED_FACE('',(#3583,#889,#890,#891,#892,#893,#894,#895,#896,
#897),#2902,.T.) ;
#12979 = ADVANCED_FACE('',(#3584,#898),#12266,.T.) ;
#12980 = ADVANCED_FACE('',(#3585,#899),#12267,.T.) ;
#12981 = ADVANCED_FACE('',(#3586),#2903,.F.) ;
#12982 = ADVANCED_FACE('',(#3587),#2904,.T.) ;
#12983 = ADVANCED_FACE('',(#3588,#900),#12268,.T.) ;
#12984 = ADVANCED_FACE('',(#3589,#901),#12269,.T.) ;
#12985 = ADVANCED_FACE('',(#3590),#12270,.T.) ;
#12986 = ADVANCED_FACE('',(#3591),#2905,.T.) ;
#12987 = ADVANCED_FACE('',(#3592),#2906,.F.) ;
#12988 = ADVANCED_FACE('',(#3593,#902),#12271,.T.) ;
#12989 = ADVANCED_FACE('',(#3594),#2907,.T.) ;
#12990 = ADVANCED_FACE('',(#3595),#2908,.T.) ;
#12991 = ADVANCED_FACE('',(#3596),#12272,.T.) ;
#12992 = ADVANCED_FACE('',(#3597),#482,.T.) ;
#12993 = ADVANCED_FACE('',(#3598),#483,.T.) ;
#12994 = ADVANCED_FACE('',(#3599),#484,.T.) ;
#12995 = ADVANCED_FACE('',(#3600),#12273,.T.) ;
#12996 = ADVANCED_FACE('',(#3601),#2909,.T.) ;
#12997 = ADVANCED_FACE('',(#3602),#2910,.T.) ;
#12998 = ADVANCED_FACE('',(#3603),#2911,.F.) ;
#12999 = ADVANCED_FACE('',(#3604),#2912,.T.) ;
#13000 = ADVANCED_FACE('',(#3605,#903),#12274,.T.) ;
#13001 = ADVANCED_FACE('',(#3606),#12275,.F.) ;
#13002 = ADVANCED_FACE('',(#3607),#12276,.F.) ;
#13003 = ADVANCED_FACE('',(#3608),#12277,.F.) ;
#13004 = ADVANCED_FACE('',(#3609),#12278,.F.) ;
#13005 = ADVANCED_FACE('',(#3610,#904),#12279,.T.) ;
#13006 = ADVANCED_FACE('',(#3611),#2913,.F.) ;
#13007 = ADVANCED_FACE('',(#3612),#2914,.T.) ;
#13008 = ADVANCED_FACE('',(#3613,#905),#12280,.T.) ;
#13009 = ADVANCED_FACE('',(#3614),#12281,.T.) ;
#13010 = ADVANCED_FACE('',(#3615),#12282,.F.) ;
#13011 = ADVANCED_FACE('',(#3616),#12283,.F.) ;
#13012 = ADVANCED_FACE('',(#3617),#12284,.F.) ;
#13013 = ADVANCED_FACE('',(#3618),#2915,.T.) ;
#13014 = ADVANCED_FACE('',(#3619),#2916,.F.) ;
#13015 = ADVANCED_FACE('',(#3620,#906),#12285,.T.) ;
#13016 = ADVANCED_FACE('',(#3621,#907),#12286,.T.) ;
#13017 = ADVANCED_FACE('',(#3622),#2917,.F.) ;
#13018 = ADVANCED_FACE('',(#3623),#2918,.F.) ;
#13019 = ADVANCED_FACE('',(#3624),#2919,.T.) ;
#13020 = ADVANCED_FACE('',(#3625,#908),#12287,.T.) ;
#13021 = ADVANCED_FACE('',(#3626,#909),#12288,.T.) ;
#13022 = ADVANCED_FACE('',(#3627),#12289,.F.) ;
#13023 = ADVANCED_FACE('',(#3628),#2920,.F.) ;
#13024 = ADVANCED_FACE('',(#3629),#2921,.F.) ;
#13025 = ADVANCED_FACE('',(#3630),#12290,.F.) ;
#13026 = ADVANCED_FACE('',(#3631),#2922,.F.) ;
#13027 = ADVANCED_FACE('',(#3632),#11,.T.) ;
#13028 = ADVANCED_FACE('',(#3633,#910),#12291,.T.) ;
#13029 = ADVANCED_FACE('',(#3634),#2923,.T.) ;
#13030 = ADVANCED_FACE('',(#3635),#12,.T.) ;
#13031 = ADVANCED_FACE('',(#3636,#911),#12292,.T.) ;
#13032 = ADVANCED_FACE('',(#3637),#2924,.F.) ;
#13033 = ADVANCED_FACE('',(#3638),#2925,.T.) ;
#13034 = ADVANCED_FACE('',(#3639,#912),#12293,.T.) ;
#13035 = ADVANCED_FACE('',(#3640,#913),#12294,.T.) ;
#13036 = ADVANCED_FACE('',(#3641),#2926,.F.) ;
#13037 = ADVANCED_FACE('',(#3642),#2927,.F.) ;
#13038 = ADVANCED_FACE('',(#3643),#2928,.F.) ;
#13039 = ADVANCED_FACE('',(#3644),#2929,.F.) ;
#13040 = ADVANCED_FACE('',(#3645),#2930,.F.) ;
#13041 = ADVANCED_FACE('',(#3646),#2931,.T.) ;
#13042 = ADVANCED_FACE('',(#3647,#914,#915,#916,#917,#918),#12295,.T.) ;
#13043 = ADVANCED_FACE('',(#3648,#919,#920,#921,#922,#923),#12296,.T.) ;
#13044 = ADVANCED_FACE('',(#3649),#2932,.F.) ;
#13045 = ADVANCED_FACE('',(#3650),#2933,.F.) ;
#13046 = ADVANCED_FACE('',(#3651),#2934,.F.) ;
#13047 = ADVANCED_FACE('',(#3652),#2935,.F.) ;
#13048 = ADVANCED_FACE('',(#3653),#2936,.F.) ;
#13049 = ADVANCED_FACE('',(#3654),#2937,.T.) ;
#13050 = ADVANCED_FACE('',(#3655,#924,#925,#926,#927,#928),#12297,.T.) ;
#13051 = ADVANCED_FACE('',(#3656,#929,#930,#931,#932,#933),#12298,.T.) ;
#13052 = ADVANCED_FACE('',(#3657),#12299,.F.) ;
#13053 = ADVANCED_FACE('',(#3658),#2938,.F.) ;
#13054 = ADVANCED_FACE('',(#3659),#2939,.F.) ;
#13055 = ADVANCED_FACE('',(#3660),#12300,.F.) ;
#13056 = ADVANCED_FACE('',(#3661),#2940,.F.) ;
#13057 = ADVANCED_FACE('',(#3662),#2941,.F.) ;
#13058 = ADVANCED_FACE('',(#3663,#934),#12301,.T.) ;
#13059 = ADVANCED_FACE('',(#3664,#935),#12302,.T.) ;
#13060 = ADVANCED_FACE('',(#3665,#936,#937),#12303,.F.) ;
#13061 = ADVANCED_FACE('',(#3666),#12304,.F.) ;
#13062 = ADVANCED_FACE('',(#3667),#12305,.F.) ;
#13063 = ADVANCED_FACE('',(#3668,#938),#12306,.T.) ;
#13064 = ADVANCED_FACE('',(#3669,#939,#940),#2942,.T.) ;
#13065 = ADVANCED_FACE('',(#3670),#2943,.F.) ;
#13066 = ADVANCED_FACE('',(#3671,#941),#12307,.T.) ;
#13067 = ADVANCED_FACE('',(#3672),#2944,.T.) ;
#13068 = ADVANCED_FACE('',(#3673),#12308,.T.) ;
#13069 = ADVANCED_FACE('',(#3674),#2945,.T.) ;
#13070 = ADVANCED_FACE('',(#3675),#12309,.T.) ;
#13071 = ADVANCED_FACE('',(#3676,#942),#12310,.T.) ;
#13072 = ADVANCED_FACE('',(#3677),#2946,.F.) ;
#13073 = ADVANCED_FACE('',(#3678),#2947,.T.) ;
#13074 = ADVANCED_FACE('',(#3679,#943),#12311,.T.) ;
#13075 = ADVANCED_FACE('',(#3680,#944),#12312,.T.) ;
#13076 = ADVANCED_FACE('',(#3681),#2948,.F.) ;
#13077 = ADVANCED_FACE('',(#3682),#12313,.F.) ;
#13078 = ADVANCED_FACE('',(#3683),#12314,.F.) ;
#13079 = ADVANCED_FACE('',(#3684,#945),#12315,.T.) ;
#13080 = ADVANCED_FACE('',(#3685),#12316,.F.) ;
#13081 = ADVANCED_FACE('',(#3686),#12317,.F.) ;
#13082 = ADVANCED_FACE('',(#3687),#12318,.F.) ;
#13083 = ADVANCED_FACE('',(#3688),#12319,.F.) ;
#13084 = ADVANCED_FACE('',(#3689,#946),#12320,.T.) ;
#13085 = ADVANCED_FACE('',(#3690),#2949,.T.) ;
#13086 = ADVANCED_FACE('',(#3691),#12321,.T.) ;
#13087 = ADVANCED_FACE('',(#3692),#12322,.F.) ;
#13088 = ADVANCED_FACE('',(#3693),#12323,.F.) ;
#13089 = ADVANCED_FACE('',(#3694),#12324,.T.) ;
#13090 = ADVANCED_FACE('',(#3695),#12325,.F.) ;
#13091 = ADVANCED_FACE('',(#3696),#12326,.F.) ;
#13092 = ADVANCED_FACE('',(#3697),#12327,.F.) ;
#13093 = ADVANCED_FACE('',(#3698),#12328,.F.) ;
#13094 = ADVANCED_FACE('',(#3699,#947),#12329,.T.) ;
#13095 = ADVANCED_FACE('',(#3700),#2950,.T.) ;
#13096 = ADVANCED_FACE('',(#3701),#12330,.T.) ;
#13097 = ADVANCED_FACE('',(#3702),#12331,.F.) ;
#13098 = ADVANCED_FACE('',(#3703),#12332,.F.) ;
#13099 = ADVANCED_FACE('',(#3704),#12333,.T.) ;
#13100 = ADVANCED_FACE('',(#3705),#12334,.F.) ;
#13101 = ADVANCED_FACE('',(#3706),#12335,.F.) ;
#13102 = ADVANCED_FACE('',(#3707),#12336,.F.) ;
#13103 = ADVANCED_FACE('',(#3708),#12337,.F.) ;
#13104 = ADVANCED_FACE('',(#3709,#948),#12338,.T.) ;
#13105 = ADVANCED_FACE('',(#3710),#2951,.F.) ;
#13106 = ADVANCED_FACE('',(#3711),#12339,.F.) ;
#13107 = ADVANCED_FACE('',(#3712),#12340,.F.) ;
#13108 = ADVANCED_FACE('',(#3713,#949),#12341,.T.) ;
#13109 = ADVANCED_FACE('',(#3714),#12342,.F.) ;
#13110 = ADVANCED_FACE('',(#3715),#12343,.F.) ;
#13111 = ADVANCED_FACE('',(#3716),#12344,.F.) ;
#13112 = ADVANCED_FACE('',(#3717),#12345,.F.) ;
#13113 = ADVANCED_FACE('',(#3718,#950),#12346,.T.) ;
#13114 = CLOSED_SHELL('',(#12347,#12348,#12349,#12350,#12351,#12352,#12353,
#12354,#12355,#12356,#12357,#12358,#12359,#12360,#12361,#12362,#12363,#12364,
#12365,#12366,#12367,#12368,#12369,#12370,#12371,#12372,#12373,#12374,#12375,
#12376,#12377,#12378,#12379,#12380,#12381,#12382,#12383,#12384,#12385,#12386,
#12387)) ;
#13115 = CLOSED_SHELL('',(#12388,#12389,#12390,#12391,#12392,#12393,#12394,
#12395,#12396,#12397,#12398,#12399,#12400,#12401,#12402,#12403,#12404,#12405,
#12406,#12407,#12408)) ;
#13116 = CLOSED_SHELL('',(#12409,#12410,#12411)) ;
#13117 = CLOSED_SHELL('',(#12412,#12413,#12414,#12415,#12416,#12417,#12418,
#12419,#12420,#12421)) ;
#13118 = CLOSED_SHELL('',(#12422,#12423,#12424,#12425,#12426,#12427,#12428,
#12429,#12430,#12431,#12432,#12433,#12434,#12435,#12436,#12437,#12438,#12439)) ;
#13119 = CLOSED_SHELL('',(#12440,#12441,#12442,#12443,#12444,#12445,#12446,
#12447,#12448,#12449,#12450,#12451,#12452,#12453,#12454,#12455,#12456,#12457,
#12458,#12459,#12460,#12461,#12462,#12463,#12464,#12465,#12466,#12467,#12468,
#12469,#12470,#12471,#12472,#12473,#12474,#12475,#12476,#12477,#12478,#12479,
#12480,#12481,#12482,#12483,#12484,#12485,#12486,#12487,#12488,#12489,#12490,
#12491,#12492,#12493,#12494,#12495,#12496,#12497,#12498,#12499,#12500,#12501,
#12502,#12503,#12504,#12505,#12506,#12507,#12508,#12509,#12510,#12511,#12512,
#12513,#12514,#12515,#12516,#12517,#12518)) ;
#13120 = CLOSED_SHELL('',(#12519,#12520,#12521,#12522)) ;
#13121 = CLOSED_SHELL('',(#12523,#12524,#12525,#12526)) ;
#13122 = CLOSED_SHELL('',(#12527,#12528,#12529,#12530)) ;
#13123 = CLOSED_SHELL('',(#12531,#12532,#12533,#12534)) ;
#13124 = CLOSED_SHELL('',(#12535,#12536,#12537,#12538)) ;
#13125 = CLOSED_SHELL('',(#12539,#12540,#12541,#12542,#12543,#12544)) ;
#13126 = CLOSED_SHELL('',(#12545,#12546,#12547,#12548,#12549,#12550,#12551,
#12552,#12553,#12554,#12555,#12556,#12557,#12558,#12559,#12560,#12561,#12562,
#12563,#12564,#12565,#12566,#12567,#12568,#12569,#12570,#12571,#12572,#12573,
#12574,#12575,#12576,#12577,#12578,#12579,#12580,#12581,#12582,#12583,#12584,
#12585,#12586,#12587,#12588,#12589,#12590,#12591,#12592,#12593,#12594,#12595,
#12596,#12597,#12598,#12599,#12600)) ;
#13127 = CLOSED_SHELL('',(#12601,#12602,#12603,#12604,#12605,#12606)) ;
#13128 = CLOSED_SHELL('',(#12607,#12608,#12609,#12610)) ;
#13129 = CLOSED_SHELL('',(#12611,#12612,#12613,#12614,#12615,#12616,#12617,
#12618,#12619,#12620)) ;
#13130 = CLOSED_SHELL('',(#12621,#12622,#12623,#12624,#12625,#12626,#12627,
#12628,#12629,#12630,#12631,#12632,#12633,#12634,#12635)) ;
#13131 = CLOSED_SHELL('',(#12636,#12637,#12638)) ;
#13132 = CLOSED_SHELL('',(#12639,#12640,#12641,#12642,#12643,#12644,#12645,
#12646,#12647,#12648,#12649,#12650,#12651,#12652,#12653,#12654,#12655,#12656,
#12657,#12658,#12659,#12660,#12661,#12662,#12663,#12664,#12665,#12666,#12667,
#12668,#12669,#12670,#12671,#12672,#12673,#12674,#12675,#12676,#12677,#12678,
#12679,#12680,#12681,#12682,#12683,#12684,#12685,#12686,#12687,#12688,#12689,
#12690,#12691,#12692,#12693,#12694,#12695,#12696,#12697,#12698,#12699,#12700,
#12701,#12702,#12703)) ;
#13133 = CLOSED_SHELL('',(#12704,#12705)) ;
#13134 = CLOSED_SHELL('',(#12706,#12707)) ;
#13135 = CLOSED_SHELL('',(#12708,#12709,#12710)) ;
#13136 = CLOSED_SHELL('',(#12711,#12712,#12713,#12714)) ;
#13137 = CLOSED_SHELL('',(#12715,#12716,#12717)) ;
#13138 = CLOSED_SHELL('',(#12718,#12719)) ;
#13139 = CLOSED_SHELL('',(#12720,#12721,#12722)) ;
#13140 = CLOSED_SHELL('',(#12723,#12724,#12725)) ;
#13141 = CLOSED_SHELL('',(#12726,#12727)) ;
#13142 = CLOSED_SHELL('',(#12728,#12729,#12730)) ;
#13143 = CLOSED_SHELL('',(#12731,#12732,#12733)) ;
#13144 = CLOSED_SHELL('',(#12734,#12735)) ;
#13145 = CLOSED_SHELL('',(#12736,#12737,#12738)) ;
#13146 = CLOSED_SHELL('',(#12739,#12740,#12741)) ;
#13147 = CLOSED_SHELL('',(#12742,#12743)) ;
#13148 = CLOSED_SHELL('',(#12744,#12745,#12746)) ;
#13149 = CLOSED_SHELL('',(#12747,#12748,#12749)) ;
#13150 = CLOSED_SHELL('',(#12750,#12751)) ;
#13151 = CLOSED_SHELL('',(#12752,#12753,#12754)) ;
#13152 = CLOSED_SHELL('',(#12755,#12756,#12757)) ;
#13153 = CLOSED_SHELL('',(#12758,#12759)) ;
#13154 = CLOSED_SHELL('',(#12760,#12761,#12762)) ;
#13155 = CLOSED_SHELL('',(#12763,#12764)) ;
#13156 = CLOSED_SHELL('',(#12765,#12766)) ;
#13157 = CLOSED_SHELL('',(#12767,#12768,#12769,#12770)) ;
#13158 = CLOSED_SHELL('',(#12771,#12772,#12773,#12774,#12775,#12776,#12777,
#12778,#12779,#12780,#12781,#12782,#12783,#12784,#12785,#12786,#12787,#12788,
#12789,#12790,#12791,#12792,#12793,#12794,#12795,#12796,#12797,#12798,#12799,
#12800,#12801,#12802,#12803,#12804,#12805,#12806,#12807,#12808,#12809)) ;
#13159 = CLOSED_SHELL('',(#12810,#12811)) ;
#13160 = CLOSED_SHELL('',(#12812,#12813)) ;
#13161 = CLOSED_SHELL('',(#12814,#12815)) ;
#13162 = CLOSED_SHELL('',(#12816,#12817)) ;
#13163 = CLOSED_SHELL('',(#12818,#12819)) ;
#13164 = CLOSED_SHELL('',(#12820,#12821)) ;
#13165 = CLOSED_SHELL('',(#12822,#12823,#12824,#12825,#12826,#12827,#12828,
#12829,#12830,#12831,#12832,#12833,#12834,#12835,#12836,#12837,#12838,#12839)) ;
#13166 = CLOSED_SHELL('',(#12840,#12841,#12842,#12843,#12844,#12845,#12846,
#12847,#12848,#12849)) ;
#13167 = CLOSED_SHELL('',(#12850,#12851,#12852,#12853,#12854,#12855,#12856,
#12857,#12858,#12859,#12860,#12861,#12862,#12863,#12864,#12865,#12866,#12867)) ;
#13168 = CLOSED_SHELL('',(#12868,#12869,#12870,#12871,#12872,#12873,#12874,
#12875,#12876,#12877,#12878,#12879,#12880,#12881,#12882,#12883,#12884,#12885,
#12886,#12887,#12888,#12889,#12890,#12891,#12892,#12893,#12894,#12895,#12896,
#12897,#12898)) ;
#13169 = CLOSED_SHELL('',(#12899,#12900,#12901,#12902,#12903,#12904,#12905,
#12906,#12907,#12908,#12909,#12910,#12911,#12912,#12913,#12914,#12915,#12916,
#12917)) ;
#13170 = CLOSED_SHELL('',(#12918,#12919,#12920)) ;
#13171 = CLOSED_SHELL('',(#12921,#12922,#12923,#12924)) ;
#13172 = CLOSED_SHELL('',(#12925,#12926,#12927,#12928,#12929,#12930,#12931,
#12932,#12933,#12934,#12935,#12936,#12937,#12938,#12939,#12940,#12941,#12942,
#12943,#12944,#12945,#12946,#12947,#12948,#12949,#12950,#12951,#12952,#12953,
#12954,#12955,#12956,#12957,#12958,#12959,#12960,#12961,#12962,#12963,#12964,
#12965,#12966,#12967,#12968,#12969,#12970,#12971,#12972,#12973,#12974,#12975,
#12976,#12977,#12978,#12979,#12980)) ;
#13173 = CLOSED_SHELL('',(#12981,#12982,#12983,#12984)) ;
#13174 = CLOSED_SHELL('',(#12985,#12986,#12987,#12988,#12989,#12990,#12991,
#12992,#12993,#12994,#12995,#12996,#12997,#12998,#12999,#13000)) ;
#13175 = CLOSED_SHELL('',(#13001,#13002,#13003,#13004,#13005,#13006,#13007,
#13008)) ;
#13176 = CLOSED_SHELL('',(#13009,#13010,#13011,#13012,#13013,#13014,#13015,
#13016)) ;
#13177 = CLOSED_SHELL('',(#13017,#13018,#13019,#13020,#13021)) ;
#13178 = CLOSED_SHELL('',(#13022,#13023,#13024,#13025,#13026,#13027,#13028,
#13029,#13030,#13031)) ;
#13179 = CLOSED_SHELL('',(#13032,#13033,#13034,#13035)) ;
#13180 = CLOSED_SHELL('',(#13036,#13037,#13038,#13039,#13040,#13041,#13042,
#13043)) ;
#13181 = CLOSED_SHELL('',(#13044,#13045,#13046,#13047,#13048,#13049,#13050,
#13051)) ;
#13182 = CLOSED_SHELL('',(#13052,#13053,#13054,#13055,#13056,#13057,#13058,
#13059,#13060,#13061,#13062,#13063,#13064,#13065,#13066)) ;
#13183 = CLOSED_SHELL('',(#13067,#13068,#13069,#13070,#13071)) ;
#13184 = CLOSED_SHELL('',(#13072,#13073,#13074,#13075)) ;
#13185 = CLOSED_SHELL('',(#13076,#13077,#13078,#13079,#13080,#13081,#13082,
#13083,#13084)) ;
#13186 = CLOSED_SHELL('',(#13085,#13086,#13087,#13088,#13089,#13090,#13091,
#13092,#13093,#13094)) ;
#13187 = CLOSED_SHELL('',(#13095,#13096,#13097,#13098,#13099,#13100,#13101,
#13102,#13103,#13104)) ;
#13188 = CLOSED_SHELL('',(#13105,#13106,#13107,#13108,#13109,#13110,#13111,
#13112,#13113)) ;
#13189 = DERIVED_UNIT_ELEMENT(#13273,1.) ;
#13190 = DERIVED_UNIT_ELEMENT(#24630,-3.) ;
#13191 = DERIVED_UNIT_ELEMENT(#13273,1.) ;
#13192 = DERIVED_UNIT_ELEMENT(#24630,-3.) ;
#13193 = DERIVED_UNIT_ELEMENT(#13273,1.) ;
#13194 = DERIVED_UNIT_ELEMENT(#24630,-3.) ;
#13195 = DERIVED_UNIT_ELEMENT(#13273,1.) ;
#13196 = DERIVED_UNIT_ELEMENT(#24630,-3.) ;
#13197 = DERIVED_UNIT_ELEMENT(#13273,1.) ;
#13198 = DERIVED_UNIT_ELEMENT(#24630,-3.) ;
#13199 = DERIVED_UNIT_ELEMENT(#13273,1.) ;
#13200 = DERIVED_UNIT_ELEMENT(#24630,-3.) ;
#13201 = DERIVED_UNIT_ELEMENT(#13273,1.) ;
#13202 = DERIVED_UNIT_ELEMENT(#24630,-3.) ;
#13203 = DERIVED_UNIT_ELEMENT(#13273,1.) ;
#13204 = DERIVED_UNIT_ELEMENT(#24630,-3.) ;
#13205 = DERIVED_UNIT_ELEMENT(#13273,1.) ;
#13206 = DERIVED_UNIT_ELEMENT(#24630,-3.) ;
#13207 = DERIVED_UNIT_ELEMENT(#13273,1.) ;
#13208 = DERIVED_UNIT_ELEMENT(#24630,-3.) ;
#13209 = DERIVED_UNIT_ELEMENT(#13273,1.) ;
#13210 = DERIVED_UNIT_ELEMENT(#24630,-3.) ;
#13211 = DERIVED_UNIT_ELEMENT(#13273,1.) ;
#13212 = DERIVED_UNIT_ELEMENT(#24630,-3.) ;
#13213 = DERIVED_UNIT_ELEMENT(#13273,1.) ;
#13214 = DERIVED_UNIT_ELEMENT(#24630,-3.) ;
#13215 = DERIVED_UNIT_ELEMENT(#13273,1.) ;
#13216 = DERIVED_UNIT_ELEMENT(#24630,-3.) ;
#13217 = DERIVED_UNIT_ELEMENT(#13273,1.) ;
#13218 = DERIVED_UNIT_ELEMENT(#24630,-3.) ;
#13219 = DERIVED_UNIT_ELEMENT(#13273,1.) ;
#13220 = DERIVED_UNIT_ELEMENT(#24630,-3.) ;
#13221 = DERIVED_UNIT_ELEMENT(#13273,1.) ;
#13222 = DERIVED_UNIT_ELEMENT(#24630,-3.) ;
#13223 = DERIVED_UNIT_ELEMENT(#13273,1.) ;
#13224 = DERIVED_UNIT_ELEMENT(#24630,-3.) ;
#13225 = DERIVED_UNIT_ELEMENT(#13273,1.) ;
#13226 = DERIVED_UNIT_ELEMENT(#24630,-3.) ;
#13227 = DERIVED_UNIT_ELEMENT(#13273,1.) ;
#13228 = DERIVED_UNIT_ELEMENT(#24630,-3.) ;
#13229 = DERIVED_UNIT_ELEMENT(#13273,1.) ;
#13230 = DERIVED_UNIT_ELEMENT(#24630,-3.) ;
#13231 = DERIVED_UNIT_ELEMENT(#13273,1.) ;
#13232 = DERIVED_UNIT_ELEMENT(#24630,-3.) ;
#13233 = DERIVED_UNIT_ELEMENT(#13273,1.) ;
#13234 = DERIVED_UNIT_ELEMENT(#24630,-3.) ;
#13235 = DERIVED_UNIT_ELEMENT(#13273,1.) ;
#13236 = DERIVED_UNIT_ELEMENT(#24630,-3.) ;
#13237 = DERIVED_UNIT_ELEMENT(#13273,1.) ;
#13238 = DERIVED_UNIT_ELEMENT(#24630,-3.) ;
#13239 = DERIVED_UNIT_ELEMENT(#13273,1.) ;
#13240 = DERIVED_UNIT_ELEMENT(#24630,-3.) ;
#13241 = DERIVED_UNIT_ELEMENT(#13273,1.) ;
#13242 = DERIVED_UNIT_ELEMENT(#24630,-3.) ;
#13243 = DERIVED_UNIT_ELEMENT(#13273,1.) ;
#13244 = DERIVED_UNIT_ELEMENT(#24630,-3.) ;
#13245 = DERIVED_UNIT_ELEMENT(#13273,1.) ;
#13246 = DERIVED_UNIT_ELEMENT(#24630,-3.) ;
#13247 = DERIVED_UNIT_ELEMENT(#13273,1.) ;
#13248 = DERIVED_UNIT_ELEMENT(#24630,-3.) ;
#13249 = DERIVED_UNIT_ELEMENT(#13273,1.) ;
#13250 = DERIVED_UNIT_ELEMENT(#24630,-3.) ;
#13251 = DERIVED_UNIT_ELEMENT(#13273,1.) ;
#13252 = DERIVED_UNIT_ELEMENT(#24630,-3.) ;
#13253 = DERIVED_UNIT_ELEMENT(#13273,1.) ;
#13254 = DERIVED_UNIT_ELEMENT(#24630,-3.) ;
#13255 = DERIVED_UNIT_ELEMENT(#13273,1.) ;
#13256 = DERIVED_UNIT_ELEMENT(#24630,-3.) ;
#13257 = DERIVED_UNIT_ELEMENT(#13273,1.) ;
#13258 = DERIVED_UNIT_ELEMENT(#24630,-3.) ;
#13259 = DERIVED_UNIT_ELEMENT(#13273,1.) ;
#13260 = DERIVED_UNIT_ELEMENT(#24630,-3.) ;
#13261 = DERIVED_UNIT_ELEMENT(#13273,1.) ;
#13262 = DERIVED_UNIT_ELEMENT(#24630,-3.) ;
#13263 = DERIVED_UNIT_ELEMENT(#13273,1.) ;
#13264 = DERIVED_UNIT_ELEMENT(#24630,-3.) ;
#13265 = DERIVED_UNIT_ELEMENT(#13273,1.) ;
#13266 = DERIVED_UNIT_ELEMENT(#24630,-3.) ;
#13267 = DERIVED_UNIT_ELEMENT(#13273,1.) ;
#13268 = DERIVED_UNIT_ELEMENT(#24630,-3.) ;
#13269 = DERIVED_UNIT_ELEMENT(#13273,1.) ;
#13270 = DERIVED_UNIT_ELEMENT(#24630,-3.) ;
#13271 = DERIVED_UNIT_ELEMENT(#13273,1.) ;
#13272 = DERIVED_UNIT_ELEMENT(#24630,-3.) ;
#13273 = (
MASS_UNIT()
NAMED_UNIT(*)
SI_UNIT(.KILO.,.GRAM.)
) ;
#13274 = DERIVED_UNIT((#13189,#13190)) ;
#13275 = DERIVED_UNIT((#13191,#13192)) ;
#13276 = DERIVED_UNIT((#13193,#13194)) ;
#13277 = DERIVED_UNIT((#13195,#13196)) ;
#13278 = DERIVED_UNIT((#13197,#13198)) ;
#13279 = DERIVED_UNIT((#13199,#13200)) ;
#13280 = DERIVED_UNIT((#13201,#13202)) ;
#13281 = DERIVED_UNIT((#13203,#13204)) ;
#13282 = DERIVED_UNIT((#13205,#13206)) ;
#13283 = DERIVED_UNIT((#13207,#13208)) ;
#13284 = DERIVED_UNIT((#13209,#13210)) ;
#13285 = DERIVED_UNIT((#13211,#13212)) ;
#13286 = DERIVED_UNIT((#13213,#13214)) ;
#13287 = DERIVED_UNIT((#13215,#13216)) ;
#13288 = DERIVED_UNIT((#13217,#13218)) ;
#13289 = DERIVED_UNIT((#13219,#13220)) ;
#13290 = DERIVED_UNIT((#13221,#13222)) ;
#13291 = DERIVED_UNIT((#13223,#13224)) ;
#13292 = DERIVED_UNIT((#13225,#13226)) ;
#13293 = DERIVED_UNIT((#13227,#13228)) ;
#13294 = DERIVED_UNIT((#13229,#13230)) ;
#13295 = DERIVED_UNIT((#13231,#13232)) ;
#13296 = DERIVED_UNIT((#13233,#13234)) ;
#13297 = DERIVED_UNIT((#13235,#13236)) ;
#13298 = DERIVED_UNIT((#13237,#13238)) ;
#13299 = DERIVED_UNIT((#13239,#13240)) ;
#13300 = DERIVED_UNIT((#13241,#13242)) ;
#13301 = DERIVED_UNIT((#13243,#13244)) ;
#13302 = DERIVED_UNIT((#13245,#13246)) ;
#13303 = DERIVED_UNIT((#13247,#13248)) ;
#13304 = DERIVED_UNIT((#13249,#13250)) ;
#13305 = DERIVED_UNIT((#13251,#13252)) ;
#13306 = DERIVED_UNIT((#13253,#13254)) ;
#13307 = DERIVED_UNIT((#13255,#13256)) ;
#13308 = DERIVED_UNIT((#13257,#13258)) ;
#13309 = DERIVED_UNIT((#13259,#13260)) ;
#13310 = DERIVED_UNIT((#13261,#13262)) ;
#13311 = DERIVED_UNIT((#13263,#13264)) ;
#13312 = DERIVED_UNIT((#13265,#13266)) ;
#13313 = DERIVED_UNIT((#13267,#13268)) ;
#13314 = DERIVED_UNIT((#13269,#13270)) ;
#13315 = DERIVED_UNIT((#13271,#13272)) ;
#13316 = MEASURE_REPRESENTATION_ITEM('density measure',
POSITIVE_RATIO_MEASURE(7850.),#13274) ;
#13317 = MEASURE_REPRESENTATION_ITEM('density measure',
POSITIVE_RATIO_MEASURE(7850.),#13275) ;
#13318 = MEASURE_REPRESENTATION_ITEM('density measure',
POSITIVE_RATIO_MEASURE(7850.),#13276) ;
#13319 = MEASURE_REPRESENTATION_ITEM('density measure',
POSITIVE_RATIO_MEASURE(7850.),#13277) ;
#13320 = MEASURE_REPRESENTATION_ITEM('density measure',
POSITIVE_RATIO_MEASURE(7850.),#13278) ;
#13321 = MEASURE_REPRESENTATION_ITEM('density measure',
POSITIVE_RATIO_MEASURE(7850.),#13279) ;
#13322 = MEASURE_REPRESENTATION_ITEM('density measure',
POSITIVE_RATIO_MEASURE(7850.),#13280) ;
#13323 = MEASURE_REPRESENTATION_ITEM('density measure',
POSITIVE_RATIO_MEASURE(7850.),#13281) ;
#13324 = MEASURE_REPRESENTATION_ITEM('density measure',
POSITIVE_RATIO_MEASURE(7850.),#13282) ;
#13325 = MEASURE_REPRESENTATION_ITEM('density measure',
POSITIVE_RATIO_MEASURE(7850.),#13283) ;
#13326 = MEASURE_REPRESENTATION_ITEM('density measure',
POSITIVE_RATIO_MEASURE(7850.),#13284) ;
#13327 = MEASURE_REPRESENTATION_ITEM('density measure',
POSITIVE_RATIO_MEASURE(7850.),#13285) ;
#13328 = MEASURE_REPRESENTATION_ITEM('density measure',
POSITIVE_RATIO_MEASURE(7850.),#13286) ;
#13329 = MEASURE_REPRESENTATION_ITEM('density measure',
POSITIVE_RATIO_MEASURE(7850.),#13287) ;
#13330 = MEASURE_REPRESENTATION_ITEM('density measure',
POSITIVE_RATIO_MEASURE(7850.),#13288) ;
#13331 = MEASURE_REPRESENTATION_ITEM('density measure',
POSITIVE_RATIO_MEASURE(7850.),#13289) ;
#13332 = MEASURE_REPRESENTATION_ITEM('density measure',
POSITIVE_RATIO_MEASURE(7850.),#13290) ;
#13333 = MEASURE_REPRESENTATION_ITEM('density measure',
POSITIVE_RATIO_MEASURE(7850.),#13291) ;
#13334 = MEASURE_REPRESENTATION_ITEM('density measure',
POSITIVE_RATIO_MEASURE(7850.),#13292) ;
#13335 = MEASURE_REPRESENTATION_ITEM('density measure',
POSITIVE_RATIO_MEASURE(7850.),#13293) ;
#13336 = MEASURE_REPRESENTATION_ITEM('density measure',
POSITIVE_RATIO_MEASURE(7850.),#13294) ;
#13337 = MEASURE_REPRESENTATION_ITEM('density measure',
POSITIVE_RATIO_MEASURE(7850.),#13295) ;
#13338 = MEASURE_REPRESENTATION_ITEM('density measure',
POSITIVE_RATIO_MEASURE(7850.),#13296) ;
#13339 = MEASURE_REPRESENTATION_ITEM('density measure',
POSITIVE_RATIO_MEASURE(7850.),#13297) ;
#13340 = MEASURE_REPRESENTATION_ITEM('density measure',
POSITIVE_RATIO_MEASURE(7850.),#13298) ;
#13341 = MEASURE_REPRESENTATION_ITEM('density measure',
POSITIVE_RATIO_MEASURE(7850.),#13299) ;
#13342 = MEASURE_REPRESENTATION_ITEM('density measure',
POSITIVE_RATIO_MEASURE(7850.),#13300) ;
#13343 = MEASURE_REPRESENTATION_ITEM('density measure',
POSITIVE_RATIO_MEASURE(7850.),#13301) ;
#13344 = MEASURE_REPRESENTATION_ITEM('density measure',
POSITIVE_RATIO_MEASURE(7850.),#13302) ;
#13345 = MEASURE_REPRESENTATION_ITEM('density measure',
POSITIVE_RATIO_MEASURE(7850.),#13303) ;
#13346 = MEASURE_REPRESENTATION_ITEM('density measure',
POSITIVE_RATIO_MEASURE(7850.),#13304) ;
#13347 = MEASURE_REPRESENTATION_ITEM('density measure',
POSITIVE_RATIO_MEASURE(7850.),#13305) ;
#13348 = MEASURE_REPRESENTATION_ITEM('density measure',
POSITIVE_RATIO_MEASURE(7850.),#13306) ;
#13349 = MEASURE_REPRESENTATION_ITEM('density measure',
POSITIVE_RATIO_MEASURE(7850.),#13307) ;
#13350 = MEASURE_REPRESENTATION_ITEM('density measure',
POSITIVE_RATIO_MEASURE(7850.),#13308) ;
#13351 = MEASURE_REPRESENTATION_ITEM('density measure',
POSITIVE_RATIO_MEASURE(7850.),#13309) ;
#13352 = MEASURE_REPRESENTATION_ITEM('density measure',
POSITIVE_RATIO_MEASURE(7850.),#13310) ;
#13353 = MEASURE_REPRESENTATION_ITEM('density measure',
POSITIVE_RATIO_MEASURE(7850.),#13311) ;
#13354 = MEASURE_REPRESENTATION_ITEM('density measure',
POSITIVE_RATIO_MEASURE(7850.),#13312) ;
#13355 = MEASURE_REPRESENTATION_ITEM('density measure',
POSITIVE_RATIO_MEASURE(7850.),#13313) ;
#13356 = MEASURE_REPRESENTATION_ITEM('density measure',
POSITIVE_RATIO_MEASURE(7850.),#13314) ;
#13357 = MEASURE_REPRESENTATION_ITEM('density measure',
POSITIVE_RATIO_MEASURE(7850.),#13315) ;
#13358 = PROPERTY_DEFINITION_REPRESENTATION(#13568,#13442) ;
#13359 = PROPERTY_DEFINITION_REPRESENTATION(#13569,#13443) ;
#13360 = PROPERTY_DEFINITION_REPRESENTATION(#13570,#13444) ;
#13361 = PROPERTY_DEFINITION_REPRESENTATION(#13571,#13445) ;
#13362 = PROPERTY_DEFINITION_REPRESENTATION(#13572,#13446) ;
#13363 = PROPERTY_DEFINITION_REPRESENTATION(#13573,#13447) ;
#13364 = PROPERTY_DEFINITION_REPRESENTATION(#13574,#13448) ;
#13365 = PROPERTY_DEFINITION_REPRESENTATION(#13575,#13449) ;
#13366 = PROPERTY_DEFINITION_REPRESENTATION(#13576,#13450) ;
#13367 = PROPERTY_DEFINITION_REPRESENTATION(#13577,#13451) ;
#13368 = PROPERTY_DEFINITION_REPRESENTATION(#13578,#13452) ;
#13369 = PROPERTY_DEFINITION_REPRESENTATION(#13579,#13453) ;
#13370 = PROPERTY_DEFINITION_REPRESENTATION(#13580,#13454) ;
#13371 = PROPERTY_DEFINITION_REPRESENTATION(#13581,#13455) ;
#13372 = PROPERTY_DEFINITION_REPRESENTATION(#13582,#13456) ;
#13373 = PROPERTY_DEFINITION_REPRESENTATION(#13583,#13457) ;
#13374 = PROPERTY_DEFINITION_REPRESENTATION(#13584,#13458) ;
#13375 = PROPERTY_DEFINITION_REPRESENTATION(#13585,#13459) ;
#13376 = PROPERTY_DEFINITION_REPRESENTATION(#13586,#13460) ;
#13377 = PROPERTY_DEFINITION_REPRESENTATION(#13587,#13461) ;
#13378 = PROPERTY_DEFINITION_REPRESENTATION(#13588,#13462) ;
#13379 = PROPERTY_DEFINITION_REPRESENTATION(#13589,#13463) ;
#13380 = PROPERTY_DEFINITION_REPRESENTATION(#13590,#13464) ;
#13381 = PROPERTY_DEFINITION_REPRESENTATION(#13591,#13465) ;
#13382 = PROPERTY_DEFINITION_REPRESENTATION(#13592,#13466) ;
#13383 = PROPERTY_DEFINITION_REPRESENTATION(#13593,#13467) ;
#13384 = PROPERTY_DEFINITION_REPRESENTATION(#13594,#13468) ;
#13385 = PROPERTY_DEFINITION_REPRESENTATION(#13595,#13469) ;
#13386 = PROPERTY_DEFINITION_REPRESENTATION(#13596,#13470) ;
#13387 = PROPERTY_DEFINITION_REPRESENTATION(#13597,#13471) ;
#13388 = PROPERTY_DEFINITION_REPRESENTATION(#13598,#13472) ;
#13389 = PROPERTY_DEFINITION_REPRESENTATION(#13599,#13473) ;
#13390 = PROPERTY_DEFINITION_REPRESENTATION(#13600,#13474) ;
#13391 = PROPERTY_DEFINITION_REPRESENTATION(#13601,#13475) ;
#13392 = PROPERTY_DEFINITION_REPRESENTATION(#13602,#13476) ;
#13393 = PROPERTY_DEFINITION_REPRESENTATION(#13603,#13477) ;
#13394 = PROPERTY_DEFINITION_REPRESENTATION(#13604,#13478) ;
#13395 = PROPERTY_DEFINITION_REPRESENTATION(#13605,#13479) ;
#13396 = PROPERTY_DEFINITION_REPRESENTATION(#13606,#13480) ;
#13397 = PROPERTY_DEFINITION_REPRESENTATION(#13607,#13481) ;
#13398 = PROPERTY_DEFINITION_REPRESENTATION(#13608,#13482) ;
#13399 = PROPERTY_DEFINITION_REPRESENTATION(#13609,#13483) ;
#13400 = PROPERTY_DEFINITION_REPRESENTATION(#13610,#13484) ;
#13401 = PROPERTY_DEFINITION_REPRESENTATION(#13611,#13485) ;
#13402 = PROPERTY_DEFINITION_REPRESENTATION(#13612,#13486) ;
#13403 = PROPERTY_DEFINITION_REPRESENTATION(#13613,#13487) ;
#13404 = PROPERTY_DEFINITION_REPRESENTATION(#13614,#13488) ;
#13405 = PROPERTY_DEFINITION_REPRESENTATION(#13615,#13489) ;
#13406 = PROPERTY_DEFINITION_REPRESENTATION(#13616,#13490) ;
#13407 = PROPERTY_DEFINITION_REPRESENTATION(#13617,#13491) ;
#13408 = PROPERTY_DEFINITION_REPRESENTATION(#13618,#13492) ;
#13409 = PROPERTY_DEFINITION_REPRESENTATION(#13619,#13493) ;
#13410 = PROPERTY_DEFINITION_REPRESENTATION(#13620,#13494) ;
#13411 = PROPERTY_DEFINITION_REPRESENTATION(#13621,#13495) ;
#13412 = PROPERTY_DEFINITION_REPRESENTATION(#13622,#13496) ;
#13413 = PROPERTY_DEFINITION_REPRESENTATION(#13623,#13497) ;
#13414 = PROPERTY_DEFINITION_REPRESENTATION(#13624,#13498) ;
#13415 = PROPERTY_DEFINITION_REPRESENTATION(#13625,#13499) ;
#13416 = PROPERTY_DEFINITION_REPRESENTATION(#13626,#13500) ;
#13417 = PROPERTY_DEFINITION_REPRESENTATION(#13627,#13501) ;
#13418 = PROPERTY_DEFINITION_REPRESENTATION(#13628,#13502) ;
#13419 = PROPERTY_DEFINITION_REPRESENTATION(#13629,#13503) ;
#13420 = PROPERTY_DEFINITION_REPRESENTATION(#13630,#13504) ;
#13421 = PROPERTY_DEFINITION_REPRESENTATION(#13631,#13505) ;
#13422 = PROPERTY_DEFINITION_REPRESENTATION(#13632,#13506) ;
#13423 = PROPERTY_DEFINITION_REPRESENTATION(#13633,#13507) ;
#13424 = PROPERTY_DEFINITION_REPRESENTATION(#13634,#13508) ;
#13425 = PROPERTY_DEFINITION_REPRESENTATION(#13635,#13509) ;
#13426 = PROPERTY_DEFINITION_REPRESENTATION(#13636,#13510) ;
#13427 = PROPERTY_DEFINITION_REPRESENTATION(#13637,#13511) ;
#13428 = PROPERTY_DEFINITION_REPRESENTATION(#13638,#13512) ;
#13429 = PROPERTY_DEFINITION_REPRESENTATION(#13639,#13513) ;
#13430 = PROPERTY_DEFINITION_REPRESENTATION(#13640,#13514) ;
#13431 = PROPERTY_DEFINITION_REPRESENTATION(#13641,#13515) ;
#13432 = PROPERTY_DEFINITION_REPRESENTATION(#13642,#13516) ;
#13433 = PROPERTY_DEFINITION_REPRESENTATION(#13643,#13517) ;
#13434 = PROPERTY_DEFINITION_REPRESENTATION(#13644,#13518) ;
#13435 = PROPERTY_DEFINITION_REPRESENTATION(#13645,#13519) ;
#13436 = PROPERTY_DEFINITION_REPRESENTATION(#13646,#13520) ;
#13437 = PROPERTY_DEFINITION_REPRESENTATION(#13647,#13521) ;
#13438 = PROPERTY_DEFINITION_REPRESENTATION(#13648,#13522) ;
#13439 = PROPERTY_DEFINITION_REPRESENTATION(#13649,#13523) ;
#13440 = PROPERTY_DEFINITION_REPRESENTATION(#13650,#13524) ;
#13441 = PROPERTY_DEFINITION_REPRESENTATION(#13651,#13525) ;
#13442 = REPRESENTATION('material name',(#13526),#24583) ;
#13443 = REPRESENTATION('density',(#13316),#24583) ;
#13444 = REPRESENTATION('material name',(#13527),#24584) ;
#13445 = REPRESENTATION('density',(#13317),#24584) ;
#13446 = REPRESENTATION('material name',(#13528),#24585) ;
#13447 = REPRESENTATION('density',(#13318),#24585) ;
#13448 = REPRESENTATION('material name',(#13529),#24586) ;
#13449 = REPRESENTATION('density',(#13319),#24586) ;
#13450 = REPRESENTATION('material name',(#13530),#24587) ;
#13451 = REPRESENTATION('density',(#13320),#24587) ;
#13452 = REPRESENTATION('material name',(#13531),#24588) ;
#13453 = REPRESENTATION('density',(#13321),#24588) ;
#13454 = REPRESENTATION('material name',(#13532),#24589) ;
#13455 = REPRESENTATION('density',(#13322),#24589) ;
#13456 = REPRESENTATION('material name',(#13533),#24590) ;
#13457 = REPRESENTATION('density',(#13323),#24590) ;
#13458 = REPRESENTATION('material name',(#13534),#24591) ;
#13459 = REPRESENTATION('density',(#13324),#24591) ;
#13460 = REPRESENTATION('material name',(#13535),#24592) ;
#13461 = REPRESENTATION('density',(#13325),#24592) ;
#13462 = REPRESENTATION('material name',(#13536),#24593) ;
#13463 = REPRESENTATION('density',(#13326),#24593) ;
#13464 = REPRESENTATION('material name',(#13537),#24594) ;
#13465 = REPRESENTATION('density',(#13327),#24594) ;
#13466 = REPRESENTATION('material name',(#13538),#24595) ;
#13467 = REPRESENTATION('density',(#13328),#24595) ;
#13468 = REPRESENTATION('material name',(#13539),#24596) ;
#13469 = REPRESENTATION('density',(#13329),#24596) ;
#13470 = REPRESENTATION('material name',(#13540),#24597) ;
#13471 = REPRESENTATION('density',(#13330),#24597) ;
#13472 = REPRESENTATION('material name',(#13541),#24598) ;
#13473 = REPRESENTATION('density',(#13331),#24598) ;
#13474 = REPRESENTATION('material name',(#13542),#24599) ;
#13475 = REPRESENTATION('density',(#13332),#24599) ;
#13476 = REPRESENTATION('material name',(#13543),#24600) ;
#13477 = REPRESENTATION('density',(#13333),#24600) ;
#13478 = REPRESENTATION('material name',(#13544),#24601) ;
#13479 = REPRESENTATION('density',(#13334),#24601) ;
#13480 = REPRESENTATION('material name',(#13545),#24603) ;
#13481 = REPRESENTATION('density',(#13335),#24603) ;
#13482 = REPRESENTATION('material name',(#13546),#24604) ;
#13483 = REPRESENTATION('density',(#13336),#24604) ;
#13484 = REPRESENTATION('material name',(#13547),#24605) ;
#13485 = REPRESENTATION('density',(#13337),#24605) ;
#13486 = REPRESENTATION('material name',(#13548),#24606) ;
#13487 = REPRESENTATION('density',(#13338),#24606) ;
#13488 = REPRESENTATION('material name',(#13549),#24607) ;
#13489 = REPRESENTATION('density',(#13339),#24607) ;
#13490 = REPRESENTATION('material name',(#13550),#24608) ;
#13491 = REPRESENTATION('density',(#13340),#24608) ;
#13492 = REPRESENTATION('material name',(#13551),#24609) ;
#13493 = REPRESENTATION('density',(#13341),#24609) ;
#13494 = REPRESENTATION('material name',(#13552),#24610) ;
#13495 = REPRESENTATION('density',(#13342),#24610) ;
#13496 = REPRESENTATION('material name',(#13553),#24611) ;
#13497 = REPRESENTATION('density',(#13343),#24611) ;
#13498 = REPRESENTATION('material name',(#13554),#24612) ;
#13499 = REPRESENTATION('density',(#13344),#24612) ;
#13500 = REPRESENTATION('material name',(#13555),#24613) ;
#13501 = REPRESENTATION('density',(#13345),#24613) ;
#13502 = REPRESENTATION('material name',(#13556),#24615) ;
#13503 = REPRESENTATION('density',(#13346),#24615) ;
#13504 = REPRESENTATION('material name',(#13557),#24616) ;
#13505 = REPRESENTATION('density',(#13347),#24616) ;
#13506 = REPRESENTATION('material name',(#13558),#24617) ;
#13507 = REPRESENTATION('density',(#13348),#24617) ;
#13508 = REPRESENTATION('material name',(#13559),#24618) ;
#13509 = REPRESENTATION('density',(#13349),#24618) ;
#13510 = REPRESENTATION('material name',(#13560),#24619) ;
#13511 = REPRESENTATION('density',(#13350),#24619) ;
#13512 = REPRESENTATION('material name',(#13561),#24620) ;
#13513 = REPRESENTATION('density',(#13351),#24620) ;
#13514 = REPRESENTATION('material name',(#13562),#24622) ;
#13515 = REPRESENTATION('density',(#13352),#24622) ;
#13516 = REPRESENTATION('material name',(#13563),#24623) ;
#13517 = REPRESENTATION('density',(#13353),#24623) ;
#13518 = REPRESENTATION('material name',(#13564),#24624) ;
#13519 = REPRESENTATION('density',(#13354),#24624) ;
#13520 = REPRESENTATION('material name',(#13565),#24625) ;
#13521 = REPRESENTATION('density',(#13355),#24625) ;
#13522 = REPRESENTATION('material name',(#13566),#24626) ;
#13523 = REPRESENTATION('density',(#13356),#24626) ;
#13524 = REPRESENTATION('material name',(#13567),#24627) ;
#13525 = REPRESENTATION('density',(#13357),#24627) ;
#13526 = DESCRIPTIVE_REPRESENTATION_ITEM('Steel','Steel') ;
#13527 = DESCRIPTIVE_REPRESENTATION_ITEM('Steel','Steel') ;
#13528 = DESCRIPTIVE_REPRESENTATION_ITEM('Steel','Steel') ;
#13529 = DESCRIPTIVE_REPRESENTATION_ITEM('Steel','Steel') ;
#13530 = DESCRIPTIVE_REPRESENTATION_ITEM('Steel','Steel') ;
#13531 = DESCRIPTIVE_REPRESENTATION_ITEM('Steel','Steel') ;
#13532 = DESCRIPTIVE_REPRESENTATION_ITEM('Steel','Steel') ;
#13533 = DESCRIPTIVE_REPRESENTATION_ITEM('Steel','Steel') ;
#13534 = DESCRIPTIVE_REPRESENTATION_ITEM('Steel','Steel') ;
#13535 = DESCRIPTIVE_REPRESENTATION_ITEM('Steel','Steel') ;
#13536 = DESCRIPTIVE_REPRESENTATION_ITEM('Steel','Steel') ;
#13537 = DESCRIPTIVE_REPRESENTATION_ITEM('Steel','Steel') ;
#13538 = DESCRIPTIVE_REPRESENTATION_ITEM('Steel','Steel') ;
#13539 = DESCRIPTIVE_REPRESENTATION_ITEM('Steel','Steel') ;
#13540 = DESCRIPTIVE_REPRESENTATION_ITEM('Steel','Steel') ;
#13541 = DESCRIPTIVE_REPRESENTATION_ITEM('Steel','Steel') ;
#13542 = DESCRIPTIVE_REPRESENTATION_ITEM('Steel','Steel') ;
#13543 = DESCRIPTIVE_REPRESENTATION_ITEM('Steel','Steel') ;
#13544 = DESCRIPTIVE_REPRESENTATION_ITEM('Steel','Steel') ;
#13545 = DESCRIPTIVE_REPRESENTATION_ITEM('Steel','Steel') ;
#13546 = DESCRIPTIVE_REPRESENTATION_ITEM('Steel','Steel') ;
#13547 = DESCRIPTIVE_REPRESENTATION_ITEM('Steel','Steel') ;
#13548 = DESCRIPTIVE_REPRESENTATION_ITEM('Steel','Steel') ;
#13549 = DESCRIPTIVE_REPRESENTATION_ITEM('Steel','Steel') ;
#13550 = DESCRIPTIVE_REPRESENTATION_ITEM('Steel','Steel') ;
#13551 = DESCRIPTIVE_REPRESENTATION_ITEM('Steel','Steel') ;
#13552 = DESCRIPTIVE_REPRESENTATION_ITEM('Steel','Steel') ;
#13553 = DESCRIPTIVE_REPRESENTATION_ITEM('Steel','Steel') ;
#13554 = DESCRIPTIVE_REPRESENTATION_ITEM('Steel','Steel') ;
#13555 = DESCRIPTIVE_REPRESENTATION_ITEM('Steel','Steel') ;
#13556 = DESCRIPTIVE_REPRESENTATION_ITEM('Steel','Steel') ;
#13557 = DESCRIPTIVE_REPRESENTATION_ITEM('Steel','Steel') ;
#13558 = DESCRIPTIVE_REPRESENTATION_ITEM('Steel','Steel') ;
#13559 = DESCRIPTIVE_REPRESENTATION_ITEM('Steel','Steel') ;
#13560 = DESCRIPTIVE_REPRESENTATION_ITEM('Steel','Steel') ;
#13561 = DESCRIPTIVE_REPRESENTATION_ITEM('Steel','Steel') ;
#13562 = DESCRIPTIVE_REPRESENTATION_ITEM('Steel','Steel') ;
#13563 = DESCRIPTIVE_REPRESENTATION_ITEM('Steel','Steel') ;
#13564 = DESCRIPTIVE_REPRESENTATION_ITEM('Steel','Steel') ;
#13565 = DESCRIPTIVE_REPRESENTATION_ITEM('Steel','Steel') ;
#13566 = DESCRIPTIVE_REPRESENTATION_ITEM('Steel','Steel') ;
#13567 = DESCRIPTIVE_REPRESENTATION_ITEM('Steel','Steel') ;
#13568 = PROPERTY_DEFINITION('material property','material name',#24841) ;
#13569 = PROPERTY_DEFINITION('material property','density of part',#24841) ;
#13570 = PROPERTY_DEFINITION('material property','material name',#24842) ;
#13571 = PROPERTY_DEFINITION('material property','density of part',#24842) ;
#13572 = PROPERTY_DEFINITION('material property','material name',#24843) ;
#13573 = PROPERTY_DEFINITION('material property','density of part',#24843) ;
#13574 = PROPERTY_DEFINITION('material property','material name',#24844) ;
#13575 = PROPERTY_DEFINITION('material property','density of part',#24844) ;
#13576 = PROPERTY_DEFINITION('material property','material name',#24845) ;
#13577 = PROPERTY_DEFINITION('material property','density of part',#24845) ;
#13578 = PROPERTY_DEFINITION('material property','material name',#24846) ;
#13579 = PROPERTY_DEFINITION('material property','density of part',#24846) ;
#13580 = PROPERTY_DEFINITION('material property','material name',#24847) ;
#13581 = PROPERTY_DEFINITION('material property','density of part',#24847) ;
#13582 = PROPERTY_DEFINITION('material property','material name',#24848) ;
#13583 = PROPERTY_DEFINITION('material property','density of part',#24848) ;
#13584 = PROPERTY_DEFINITION('material property','material name',#24849) ;
#13585 = PROPERTY_DEFINITION('material property','density of part',#24849) ;
#13586 = PROPERTY_DEFINITION('material property','material name',#24850) ;
#13587 = PROPERTY_DEFINITION('material property','density of part',#24850) ;
#13588 = PROPERTY_DEFINITION('material property','material name',#24851) ;
#13589 = PROPERTY_DEFINITION('material property','density of part',#24851) ;
#13590 = PROPERTY_DEFINITION('material property','material name',#24852) ;
#13591 = PROPERTY_DEFINITION('material property','density of part',#24852) ;
#13592 = PROPERTY_DEFINITION('material property','material name',#24853) ;
#13593 = PROPERTY_DEFINITION('material property','density of part',#24853) ;
#13594 = PROPERTY_DEFINITION('material property','material name',#24854) ;
#13595 = PROPERTY_DEFINITION('material property','density of part',#24854) ;
#13596 = PROPERTY_DEFINITION('material property','material name',#24855) ;
#13597 = PROPERTY_DEFINITION('material property','density of part',#24855) ;
#13598 = PROPERTY_DEFINITION('material property','material name',#24856) ;
#13599 = PROPERTY_DEFINITION('material property','density of part',#24856) ;
#13600 = PROPERTY_DEFINITION('material property','material name',#24857) ;
#13601 = PROPERTY_DEFINITION('material property','density of part',#24857) ;
#13602 = PROPERTY_DEFINITION('material property','material name',#24858) ;
#13603 = PROPERTY_DEFINITION('material property','density of part',#24858) ;
#13604 = PROPERTY_DEFINITION('material property','material name',#24859) ;
#13605 = PROPERTY_DEFINITION('material property','density of part',#24859) ;
#13606 = PROPERTY_DEFINITION('material property','material name',#24861) ;
#13607 = PROPERTY_DEFINITION('material property','density of part',#24861) ;
#13608 = PROPERTY_DEFINITION('material property','material name',#24862) ;
#13609 = PROPERTY_DEFINITION('material property','density of part',#24862) ;
#13610 = PROPERTY_DEFINITION('material property','material name',#24863) ;
#13611 = PROPERTY_DEFINITION('material property','density of part',#24863) ;
#13612 = PROPERTY_DEFINITION('material property','material name',#24864) ;
#13613 = PROPERTY_DEFINITION('material property','density of part',#24864) ;
#13614 = PROPERTY_DEFINITION('material property','material name',#24865) ;
#13615 = PROPERTY_DEFINITION('material property','density of part',#24865) ;
#13616 = PROPERTY_DEFINITION('material property','material name',#24866) ;
#13617 = PROPERTY_DEFINITION('material property','density of part',#24866) ;
#13618 = PROPERTY_DEFINITION('material property','material name',#24867) ;
#13619 = PROPERTY_DEFINITION('material property','density of part',#24867) ;
#13620 = PROPERTY_DEFINITION('material property','material name',#24868) ;
#13621 = PROPERTY_DEFINITION('material property','density of part',#24868) ;
#13622 = PROPERTY_DEFINITION('material property','material name',#24869) ;
#13623 = PROPERTY_DEFINITION('material property','density of part',#24869) ;
#13624 = PROPERTY_DEFINITION('material property','material name',#24870) ;
#13625 = PROPERTY_DEFINITION('material property','density of part',#24870) ;
#13626 = PROPERTY_DEFINITION('material property','material name',#24871) ;
#13627 = PROPERTY_DEFINITION('material property','density of part',#24871) ;
#13628 = PROPERTY_DEFINITION('material property','material name',#24873) ;
#13629 = PROPERTY_DEFINITION('material property','density of part',#24873) ;
#13630 = PROPERTY_DEFINITION('material property','material name',#24874) ;
#13631 = PROPERTY_DEFINITION('material property','density of part',#24874) ;
#13632 = PROPERTY_DEFINITION('material property','material name',#24875) ;
#13633 = PROPERTY_DEFINITION('material property','density of part',#24875) ;
#13634 = PROPERTY_DEFINITION('material property','material name',#24876) ;
#13635 = PROPERTY_DEFINITION('material property','density of part',#24876) ;
#13636 = PROPERTY_DEFINITION('material property','material name',#24877) ;
#13637 = PROPERTY_DEFINITION('material property','density of part',#24877) ;
#13638 = PROPERTY_DEFINITION('material property','material name',#24878) ;
#13639 = PROPERTY_DEFINITION('material property','density of part',#24878) ;
#13640 = PROPERTY_DEFINITION('material property','material name',#24880) ;
#13641 = PROPERTY_DEFINITION('material property','density of part',#24880) ;
#13642 = PROPERTY_DEFINITION('material property','material name',#24881) ;
#13643 = PROPERTY_DEFINITION('material property','density of part',#24881) ;
#13644 = PROPERTY_DEFINITION('material property','material name',#24882) ;
#13645 = PROPERTY_DEFINITION('material property','density of part',#24882) ;
#13646 = PROPERTY_DEFINITION('material property','material name',#24883) ;
#13647 = PROPERTY_DEFINITION('material property','density of part',#24883) ;
#13648 = PROPERTY_DEFINITION('material property','material name',#24884) ;
#13649 = PROPERTY_DEFINITION('material property','density of part',#24884) ;
#13650 = PROPERTY_DEFINITION('material property','material name',#24885) ;
#13651 = PROPERTY_DEFINITION('material property','density of part',#24885) ;
#13652 = AXIS2_PLACEMENT_3D('',#19702,#15390,#15391) ;
#13653 = AXIS2_PLACEMENT_3D('',#19703,#15392,#15393) ;
#13654 = AXIS2_PLACEMENT_3D('',#19704,#15394,#15395) ;
#13655 = AXIS2_PLACEMENT_3D('',#19705,#15396,#15397) ;
#13656 = AXIS2_PLACEMENT_3D('',#19708,#15398,#15399) ;
#13657 = AXIS2_PLACEMENT_3D('',#19710,#15400,#15401) ;
#13658 = AXIS2_PLACEMENT_3D('',#19711,#15402,#15403) ;
#13659 = AXIS2_PLACEMENT_3D('',#19712,#15404,#15405) ;
#13660 = AXIS2_PLACEMENT_3D('',#19714,#15406,#15407) ;
#13661 = AXIS2_PLACEMENT_3D('',#19719,#15410,#15411) ;
#13662 = AXIS2_PLACEMENT_3D('',#19721,#15413,#15414) ;
#13663 = AXIS2_PLACEMENT_3D('',#19723,#15415,#15416) ;
#13664 = AXIS2_PLACEMENT_3D('',#19727,#15418,#15419) ;
#13665 = AXIS2_PLACEMENT_3D('',#19731,#15421,#15422) ;
#13666 = AXIS2_PLACEMENT_3D('',#19734,#15424,#15425) ;
#13667 = AXIS2_PLACEMENT_3D('',#19736,#15426,#15427) ;
#13668 = AXIS2_PLACEMENT_3D('',#19740,#15429,#15430) ;
#13669 = AXIS2_PLACEMENT_3D('',#19743,#15432,#15433) ;
#13670 = AXIS2_PLACEMENT_3D('',#19806,#15436,#15437) ;
#13671 = AXIS2_PLACEMENT_3D('',#19808,#15438,#15439) ;
#13672 = AXIS2_PLACEMENT_3D('',#19811,#15441,#15442) ;
#13673 = AXIS2_PLACEMENT_3D('',#19812,#15443,#15444) ;
#13674 = AXIS2_PLACEMENT_3D('',#19813,#15445,#15446) ;
#13675 = AXIS2_PLACEMENT_3D('',#19814,#15447,#15448) ;
#13676 = AXIS2_PLACEMENT_3D('',#19815,#15449,#15450) ;
#13677 = AXIS2_PLACEMENT_3D('',#19817,#15451,#15452) ;
#13678 = AXIS2_PLACEMENT_3D('',#19818,#15453,#15454) ;
#13679 = AXIS2_PLACEMENT_3D('',#19820,#15455,#15456) ;
#13680 = AXIS2_PLACEMENT_3D('',#19821,#15457,#15458) ;
#13681 = AXIS2_PLACEMENT_3D('',#19823,#15459,#15460) ;
#13682 = AXIS2_PLACEMENT_3D('',#19826,#15462,#15463) ;
#13683 = AXIS2_PLACEMENT_3D('',#19827,#15464,#15465) ;
#13684 = AXIS2_PLACEMENT_3D('',#19829,#15466,#15467) ;
#13685 = AXIS2_PLACEMENT_3D('',#19832,#15469,#15470) ;
#13686 = AXIS2_PLACEMENT_3D('',#19833,#15471,#15472) ;
#13687 = AXIS2_PLACEMENT_3D('',#19835,#15473,#15474) ;
#13688 = AXIS2_PLACEMENT_3D('',#19838,#15476,#15477) ;
#13689 = AXIS2_PLACEMENT_3D('',#19839,#15478,#15479) ;
#13690 = AXIS2_PLACEMENT_3D('',#19841,#15480,#15481) ;
#13691 = AXIS2_PLACEMENT_3D('',#19844,#15483,#15484) ;
#13692 = AXIS2_PLACEMENT_3D('',#19845,#15485,#15486) ;
#13693 = AXIS2_PLACEMENT_3D('',#19847,#15487,#15488) ;
#13694 = AXIS2_PLACEMENT_3D('',#19850,#15490,#15491) ;
#13695 = AXIS2_PLACEMENT_3D('',#19851,#15492,#15493) ;
#13696 = AXIS2_PLACEMENT_3D('',#19853,#15494,#15495) ;
#13697 = AXIS2_PLACEMENT_3D('',#19856,#15497,#15498) ;
#13698 = AXIS2_PLACEMENT_3D('',#19857,#15499,#15500) ;
#13699 = AXIS2_PLACEMENT_3D('',#19870,#15507,#15508) ;
#13700 = AXIS2_PLACEMENT_3D('',#19876,#15512,#15513) ;
#13701 = AXIS2_PLACEMENT_3D('',#19878,#15514,#15515) ;
#13702 = AXIS2_PLACEMENT_3D('',#19880,#15517,#15518) ;
#13703 = AXIS2_PLACEMENT_3D('',#19886,#15522,#15523) ;
#13704 = AXIS2_PLACEMENT_3D('',#19888,#15525,#15526) ;
#13705 = AXIS2_PLACEMENT_3D('',#19890,#15527,#15528) ;
#13706 = AXIS2_PLACEMENT_3D('',#19892,#15530,#15531) ;
#13707 = AXIS2_PLACEMENT_3D('',#19896,#15534,#15535) ;
#13708 = AXIS2_PLACEMENT_3D('',#19898,#15536,#15537) ;
#13709 = AXIS2_PLACEMENT_3D('',#19901,#15539,#15540) ;
#13710 = AXIS2_PLACEMENT_3D('',#19903,#15541,#15542) ;
#13711 = AXIS2_PLACEMENT_3D('',#19907,#15544,#15545) ;
#13712 = AXIS2_PLACEMENT_3D('',#19910,#15547,#15548) ;
#13713 = AXIS2_PLACEMENT_3D('',#19965,#15549,#15550) ;
#13714 = AXIS2_PLACEMENT_3D('',#19967,#15551,#15552) ;
#13715 = AXIS2_PLACEMENT_3D('',#19969,#15554,#15555) ;
#13716 = AXIS2_PLACEMENT_3D('',#19970,#15556,#15557) ;
#13717 = AXIS2_PLACEMENT_3D('',#19973,#15559,#15560) ;
#13718 = AXIS2_PLACEMENT_3D('',#19974,#15561,#15562) ;
#13719 = AXIS2_PLACEMENT_3D('',#19975,#15563,#15564) ;
#13720 = AXIS2_PLACEMENT_3D('',#19976,#15565,#15566) ;
#13721 = AXIS2_PLACEMENT_3D('',#19977,#15567,#15568) ;
#13722 = AXIS2_PLACEMENT_3D('',#19978,#15569,#15570) ;
#13723 = AXIS2_PLACEMENT_3D('',#19979,#15571,#15572) ;
#13724 = AXIS2_PLACEMENT_3D('',#19980,#15573,#15574) ;
#13725 = AXIS2_PLACEMENT_3D('',#19982,#15575,#15576) ;
#13726 = AXIS2_PLACEMENT_3D('',#19984,#15578,#15579) ;
#13727 = AXIS2_PLACEMENT_3D('',#19985,#15580,#15581) ;
#13728 = AXIS2_PLACEMENT_3D('',#19986,#15582,#15583) ;
#13729 = AXIS2_PLACEMENT_3D('',#19988,#15584,#15585) ;
#13730 = AXIS2_PLACEMENT_3D('',#19991,#15587,#15588) ;
#13731 = AXIS2_PLACEMENT_3D('',#19992,#15589,#15590) ;
#13732 = AXIS2_PLACEMENT_3D('',#19993,#15591,#15592) ;
#13733 = AXIS2_PLACEMENT_3D('',#19994,#15593,#15594) ;
#13734 = AXIS2_PLACEMENT_3D('',#19996,#15595,#15596) ;
#13735 = AXIS2_PLACEMENT_3D('',#19997,#15597,#15598) ;
#13736 = AXIS2_PLACEMENT_3D('',#19999,#15599,#15600) ;
#13737 = AXIS2_PLACEMENT_3D('',#20002,#15602,#15603) ;
#13738 = AXIS2_PLACEMENT_3D('',#20003,#15604,#15605) ;
#13739 = AXIS2_PLACEMENT_3D('',#20005,#15606,#15607) ;
#13740 = AXIS2_PLACEMENT_3D('',#20008,#15609,#15610) ;
#13741 = AXIS2_PLACEMENT_3D('',#20009,#15611,#15612) ;
#13742 = AXIS2_PLACEMENT_3D('',#20010,#15613,#15614) ;
#13743 = AXIS2_PLACEMENT_3D('',#20012,#15615,#15616) ;
#13744 = AXIS2_PLACEMENT_3D('',#20015,#15618,#15619) ;
#13745 = AXIS2_PLACEMENT_3D('',#20016,#15620,#15621) ;
#13746 = AXIS2_PLACEMENT_3D('',#20017,#15622,#15623) ;
#13747 = AXIS2_PLACEMENT_3D('',#20019,#15624,#15625) ;
#13748 = AXIS2_PLACEMENT_3D('',#20021,#15627,#15628) ;
#13749 = AXIS2_PLACEMENT_3D('',#20022,#15629,#15630) ;
#13750 = AXIS2_PLACEMENT_3D('',#20025,#15632,#15633) ;
#13751 = AXIS2_PLACEMENT_3D('',#20026,#15634,#15635) ;
#13752 = AXIS2_PLACEMENT_3D('',#20027,#15636,#15637) ;
#13753 = AXIS2_PLACEMENT_3D('',#20028,#15638,#15639) ;
#13754 = AXIS2_PLACEMENT_3D('',#20029,#15640,#15641) ;
#13755 = AXIS2_PLACEMENT_3D('',#20031,#15642,#15643) ;
#13756 = AXIS2_PLACEMENT_3D('',#20034,#15645,#15646) ;
#13757 = AXIS2_PLACEMENT_3D('',#20035,#15647,#15648) ;
#13758 = AXIS2_PLACEMENT_3D('',#20037,#15649,#15650) ;
#13759 = AXIS2_PLACEMENT_3D('',#20040,#15652,#15653) ;
#13760 = AXIS2_PLACEMENT_3D('',#20041,#15654,#15655) ;
#13761 = AXIS2_PLACEMENT_3D('',#20043,#15656,#15657) ;
#13762 = AXIS2_PLACEMENT_3D('',#20046,#15659,#15660) ;
#13763 = AXIS2_PLACEMENT_3D('',#20047,#15661,#15662) ;
#13764 = AXIS2_PLACEMENT_3D('',#20049,#15663,#15664) ;
#13765 = AXIS2_PLACEMENT_3D('',#20052,#15666,#15667) ;
#13766 = AXIS2_PLACEMENT_3D('',#20053,#15668,#15669) ;
#13767 = AXIS2_PLACEMENT_3D('',#20055,#15670,#15671) ;
#13768 = AXIS2_PLACEMENT_3D('',#20058,#15673,#15674) ;
#13769 = AXIS2_PLACEMENT_3D('',#20059,#15675,#15676) ;
#13770 = AXIS2_PLACEMENT_3D('',#20061,#15677,#15678) ;
#13771 = AXIS2_PLACEMENT_3D('',#20064,#15680,#15681) ;
#13772 = AXIS2_PLACEMENT_3D('',#20065,#15682,#15683) ;
#13773 = AXIS2_PLACEMENT_3D('',#20067,#15684,#15685) ;
#13774 = AXIS2_PLACEMENT_3D('',#20070,#15687,#15688) ;
#13775 = AXIS2_PLACEMENT_3D('',#20071,#15689,#15690) ;
#13776 = AXIS2_PLACEMENT_3D('',#20073,#15691,#15692) ;
#13777 = AXIS2_PLACEMENT_3D('',#20076,#15694,#15695) ;
#13778 = AXIS2_PLACEMENT_3D('',#20077,#15696,#15697) ;
#13779 = AXIS2_PLACEMENT_3D('',#20079,#15698,#15699) ;
#13780 = AXIS2_PLACEMENT_3D('',#20082,#15701,#15702) ;
#13781 = AXIS2_PLACEMENT_3D('',#20083,#15703,#15704) ;
#13782 = AXIS2_PLACEMENT_3D('',#20084,#15705,#15706) ;
#13783 = AXIS2_PLACEMENT_3D('',#20086,#15707,#15708) ;
#13784 = AXIS2_PLACEMENT_3D('',#20089,#15710,#15711) ;
#13785 = AXIS2_PLACEMENT_3D('',#20090,#15712,#15713) ;
#13786 = AXIS2_PLACEMENT_3D('',#20092,#15714,#15715) ;
#13787 = AXIS2_PLACEMENT_3D('',#20095,#15717,#15718) ;
#13788 = AXIS2_PLACEMENT_3D('',#20096,#15719,#15720) ;
#13789 = AXIS2_PLACEMENT_3D('',#20097,#15721,#15722) ;
#13790 = AXIS2_PLACEMENT_3D('',#20099,#15723,#15724) ;
#13791 = AXIS2_PLACEMENT_3D('',#20102,#15726,#15727) ;
#13792 = AXIS2_PLACEMENT_3D('',#20103,#15728,#15729) ;
#13793 = AXIS2_PLACEMENT_3D('',#20105,#15730,#15731) ;
#13794 = AXIS2_PLACEMENT_3D('',#20106,#15732,#15733) ;
#13795 = AXIS2_PLACEMENT_3D('',#20108,#15734,#15735) ;
#13796 = AXIS2_PLACEMENT_3D('',#20110,#15737,#15738) ;
#13797 = AXIS2_PLACEMENT_3D('',#20112,#15739,#15740) ;
#13798 = AXIS2_PLACEMENT_3D('',#20115,#15742,#15743) ;
#13799 = AXIS2_PLACEMENT_3D('',#20116,#15744,#15745) ;
#13800 = AXIS2_PLACEMENT_3D('',#20117,#15746,#15747) ;
#13801 = AXIS2_PLACEMENT_3D('',#20119,#15748,#15749) ;
#13802 = AXIS2_PLACEMENT_3D('',#20122,#15751,#15752) ;
#13803 = AXIS2_PLACEMENT_3D('',#20123,#15753,#15754) ;
#13804 = AXIS2_PLACEMENT_3D('',#20124,#15755,#15756) ;
#13805 = AXIS2_PLACEMENT_3D('',#20125,#15757,#15758) ;
#13806 = AXIS2_PLACEMENT_3D('',#20126,#15759,#15760) ;
#13807 = AXIS2_PLACEMENT_3D('',#20128,#15761,#15762) ;
#13808 = AXIS2_PLACEMENT_3D('',#20131,#15764,#15765) ;
#13809 = AXIS2_PLACEMENT_3D('',#20132,#15766,#15767) ;
#13810 = AXIS2_PLACEMENT_3D('',#20133,#15768,#15769) ;
#13811 = AXIS2_PLACEMENT_3D('',#20134,#15770,#15771) ;
#13812 = AXIS2_PLACEMENT_3D('',#20135,#15772,#15773) ;
#13813 = AXIS2_PLACEMENT_3D('',#20137,#15774,#15775) ;
#13814 = AXIS2_PLACEMENT_3D('',#20140,#15777,#15778) ;
#13815 = AXIS2_PLACEMENT_3D('',#20141,#15779,#15780) ;
#13816 = AXIS2_PLACEMENT_3D('',#20143,#15781,#15782) ;
#13817 = AXIS2_PLACEMENT_3D('',#20146,#15784,#15785) ;
#13818 = AXIS2_PLACEMENT_3D('',#20147,#15786,#15787) ;
#13819 = AXIS2_PLACEMENT_3D('',#20149,#15788,#15789) ;
#13820 = AXIS2_PLACEMENT_3D('',#20152,#15791,#15792) ;
#13821 = AXIS2_PLACEMENT_3D('',#20153,#15793,#15794) ;
#13822 = AXIS2_PLACEMENT_3D('',#20155,#15795,#15796) ;
#13823 = AXIS2_PLACEMENT_3D('',#20158,#15798,#15799) ;
#13824 = AXIS2_PLACEMENT_3D('',#20159,#15800,#15801) ;
#13825 = AXIS2_PLACEMENT_3D('',#20161,#15802,#15803) ;
#13826 = AXIS2_PLACEMENT_3D('',#20164,#15805,#15806) ;
#13827 = AXIS2_PLACEMENT_3D('',#20165,#15807,#15808) ;
#13828 = AXIS2_PLACEMENT_3D('',#20167,#15809,#15810) ;
#13829 = AXIS2_PLACEMENT_3D('',#20170,#15812,#15813) ;
#13830 = AXIS2_PLACEMENT_3D('',#20171,#15814,#15815) ;
#13831 = AXIS2_PLACEMENT_3D('',#20173,#15816,#15817) ;
#13832 = AXIS2_PLACEMENT_3D('',#20176,#15819,#15820) ;
#13833 = AXIS2_PLACEMENT_3D('',#20177,#15821,#15822) ;
#13834 = AXIS2_PLACEMENT_3D('',#20179,#15823,#15824) ;
#13835 = AXIS2_PLACEMENT_3D('',#20182,#15826,#15827) ;
#13836 = AXIS2_PLACEMENT_3D('',#20183,#15828,#15829) ;
#13837 = AXIS2_PLACEMENT_3D('',#20184,#15830,#15831) ;
#13838 = AXIS2_PLACEMENT_3D('',#20185,#15832,#15833) ;
#13839 = AXIS2_PLACEMENT_3D('',#20186,#15834,#15835) ;
#13840 = AXIS2_PLACEMENT_3D('',#20195,#15840,#15841) ;
#13841 = AXIS2_PLACEMENT_3D('',#20197,#15842,#15843) ;
#13842 = AXIS2_PLACEMENT_3D('',#20201,#15846,#15847) ;
#13843 = AXIS2_PLACEMENT_3D('',#20207,#15851,#15852) ;
#13844 = AXIS2_PLACEMENT_3D('',#20209,#15854,#15855) ;
#13845 = AXIS2_PLACEMENT_3D('',#20211,#15856,#15857) ;
#13846 = AXIS2_PLACEMENT_3D('',#20214,#15859,#15860) ;
#13847 = AXIS2_PLACEMENT_3D('',#20215,#15861,#15862) ;
#13848 = AXIS2_PLACEMENT_3D('',#20216,#15863,#15864) ;
#13849 = AXIS2_PLACEMENT_3D('',#20218,#15865,#15866) ;
#13850 = AXIS2_PLACEMENT_3D('',#20221,#15868,#15869) ;
#13851 = AXIS2_PLACEMENT_3D('',#20222,#15870,#15871) ;
#13852 = AXIS2_PLACEMENT_3D('',#20223,#15872,#15873) ;
#13853 = AXIS2_PLACEMENT_3D('',#20225,#15874,#15875) ;
#13854 = AXIS2_PLACEMENT_3D('',#20226,#15876,#15877) ;
#13855 = AXIS2_PLACEMENT_3D('',#20228,#15878,#15879) ;
#13856 = AXIS2_PLACEMENT_3D('',#20230,#15881,#15882) ;
#13857 = AXIS2_PLACEMENT_3D('',#20232,#15883,#15884) ;
#13858 = AXIS2_PLACEMENT_3D('',#20235,#15886,#15887) ;
#13859 = AXIS2_PLACEMENT_3D('',#20236,#15888,#15889) ;
#13860 = AXIS2_PLACEMENT_3D('',#20238,#15890,#15891) ;
#13861 = AXIS2_PLACEMENT_3D('',#20241,#15893,#15894) ;
#13862 = AXIS2_PLACEMENT_3D('',#20242,#15895,#15896) ;
#13863 = AXIS2_PLACEMENT_3D('',#20244,#15897,#15898) ;
#13864 = AXIS2_PLACEMENT_3D('',#20247,#15900,#15901) ;
#13865 = AXIS2_PLACEMENT_3D('',#20248,#15902,#15903) ;
#13866 = AXIS2_PLACEMENT_3D('',#20250,#15904,#15905) ;
#13867 = AXIS2_PLACEMENT_3D('',#20251,#15906,#15907) ;
#13868 = AXIS2_PLACEMENT_3D('',#20253,#15908,#15909) ;
#13869 = AXIS2_PLACEMENT_3D('',#20255,#15911,#15912) ;
#13870 = AXIS2_PLACEMENT_3D('',#20257,#15913,#15914) ;
#13871 = AXIS2_PLACEMENT_3D('',#20260,#15916,#15917) ;
#13872 = AXIS2_PLACEMENT_3D('',#20261,#15918,#15919) ;
#13873 = AXIS2_PLACEMENT_3D('',#20262,#15920,#15921) ;
#13874 = AXIS2_PLACEMENT_3D('',#20263,#15922,#15923) ;
#13875 = AXIS2_PLACEMENT_3D('',#20264,#15924,#15925) ;
#13876 = AXIS2_PLACEMENT_3D('',#20265,#15926,#15927) ;
#13877 = AXIS2_PLACEMENT_3D('',#20267,#15928,#15929) ;
#13878 = AXIS2_PLACEMENT_3D('',#20270,#15931,#15932) ;
#13879 = AXIS2_PLACEMENT_3D('',#20271,#15933,#15934) ;
#13880 = AXIS2_PLACEMENT_3D('',#20272,#15935,#15936) ;
#13881 = AXIS2_PLACEMENT_3D('',#20274,#15937,#15938) ;
#13882 = AXIS2_PLACEMENT_3D('',#20277,#15940,#15941) ;
#13883 = AXIS2_PLACEMENT_3D('',#20278,#15942,#15943) ;
#13884 = AXIS2_PLACEMENT_3D('',#20279,#15944,#15945) ;
#13885 = AXIS2_PLACEMENT_3D('',#20281,#15946,#15947) ;
#13886 = AXIS2_PLACEMENT_3D('',#20284,#15949,#15950) ;
#13887 = AXIS2_PLACEMENT_3D('',#20285,#15951,#15952) ;
#13888 = AXIS2_PLACEMENT_3D('',#20286,#15953,#15954) ;
#13889 = AXIS2_PLACEMENT_3D('',#20288,#15955,#15956) ;
#13890 = AXIS2_PLACEMENT_3D('',#20291,#15958,#15959) ;
#13891 = AXIS2_PLACEMENT_3D('',#20292,#15960,#15961) ;
#13892 = AXIS2_PLACEMENT_3D('',#20293,#15962,#15963) ;
#13893 = AXIS2_PLACEMENT_3D('',#20295,#15964,#15965) ;
#13894 = AXIS2_PLACEMENT_3D('',#20298,#15967,#15968) ;
#13895 = AXIS2_PLACEMENT_3D('',#20299,#15969,#15970) ;
#13896 = AXIS2_PLACEMENT_3D('',#20300,#15971,#15972) ;
#13897 = AXIS2_PLACEMENT_3D('',#20302,#15973,#15974) ;
#13898 = AXIS2_PLACEMENT_3D('',#20305,#15976,#15977) ;
#13899 = AXIS2_PLACEMENT_3D('',#20306,#15978,#15979) ;
#13900 = AXIS2_PLACEMENT_3D('',#20307,#15980,#15981) ;
#13901 = AXIS2_PLACEMENT_3D('',#20309,#15982,#15983) ;
#13902 = AXIS2_PLACEMENT_3D('',#20312,#15985,#15986) ;
#13903 = AXIS2_PLACEMENT_3D('',#20313,#15987,#15988) ;
#13904 = AXIS2_PLACEMENT_3D('',#20314,#15989,#15990) ;
#13905 = AXIS2_PLACEMENT_3D('',#20316,#15991,#15992) ;
#13906 = AXIS2_PLACEMENT_3D('',#20319,#15994,#15995) ;
#13907 = AXIS2_PLACEMENT_3D('',#20320,#15996,#15997) ;
#13908 = AXIS2_PLACEMENT_3D('',#20321,#15998,#15999) ;
#13909 = AXIS2_PLACEMENT_3D('',#20323,#16000,#16001) ;
#13910 = AXIS2_PLACEMENT_3D('',#20326,#16003,#16004) ;
#13911 = AXIS2_PLACEMENT_3D('',#20327,#16005,#16006) ;
#13912 = AXIS2_PLACEMENT_3D('',#20328,#16007,#16008) ;
#13913 = AXIS2_PLACEMENT_3D('',#20330,#16009,#16010) ;
#13914 = AXIS2_PLACEMENT_3D('',#20333,#16012,#16013) ;
#13915 = AXIS2_PLACEMENT_3D('',#20334,#16014,#16015) ;
#13916 = AXIS2_PLACEMENT_3D('',#20335,#16016,#16017) ;
#13917 = AXIS2_PLACEMENT_3D('',#20337,#16018,#16019) ;
#13918 = AXIS2_PLACEMENT_3D('',#20340,#16021,#16022) ;
#13919 = AXIS2_PLACEMENT_3D('',#20341,#16023,#16024) ;
#13920 = AXIS2_PLACEMENT_3D('',#20342,#16025,#16026) ;
#13921 = AXIS2_PLACEMENT_3D('',#20344,#16027,#16028) ;
#13922 = AXIS2_PLACEMENT_3D('',#20347,#16030,#16031) ;
#13923 = AXIS2_PLACEMENT_3D('',#20348,#16032,#16033) ;
#13924 = AXIS2_PLACEMENT_3D('',#20349,#16034,#16035) ;
#13925 = AXIS2_PLACEMENT_3D('',#20351,#16036,#16037) ;
#13926 = AXIS2_PLACEMENT_3D('',#20354,#16039,#16040) ;
#13927 = AXIS2_PLACEMENT_3D('',#20355,#16041,#16042) ;
#13928 = AXIS2_PLACEMENT_3D('',#20356,#16043,#16044) ;
#13929 = AXIS2_PLACEMENT_3D('',#20358,#16045,#16046) ;
#13930 = AXIS2_PLACEMENT_3D('',#20361,#16048,#16049) ;
#13931 = AXIS2_PLACEMENT_3D('',#20362,#16050,#16051) ;
#13932 = AXIS2_PLACEMENT_3D('',#20363,#16052,#16053) ;
#13933 = AXIS2_PLACEMENT_3D('',#20365,#16054,#16055) ;
#13934 = AXIS2_PLACEMENT_3D('',#20368,#16057,#16058) ;
#13935 = AXIS2_PLACEMENT_3D('',#20369,#16059,#16060) ;
#13936 = AXIS2_PLACEMENT_3D('',#20370,#16061,#16062) ;
#13937 = AXIS2_PLACEMENT_3D('',#20372,#16063,#16064) ;
#13938 = AXIS2_PLACEMENT_3D('',#20375,#16066,#16067) ;
#13939 = AXIS2_PLACEMENT_3D('',#20376,#16068,#16069) ;
#13940 = AXIS2_PLACEMENT_3D('',#20377,#16070,#16071) ;
#13941 = AXIS2_PLACEMENT_3D('',#20379,#16072,#16073) ;
#13942 = AXIS2_PLACEMENT_3D('',#20382,#16075,#16076) ;
#13943 = AXIS2_PLACEMENT_3D('',#20383,#16077,#16078) ;
#13944 = AXIS2_PLACEMENT_3D('',#20384,#16079,#16080) ;
#13945 = AXIS2_PLACEMENT_3D('',#20386,#16081,#16082) ;
#13946 = AXIS2_PLACEMENT_3D('',#20389,#16084,#16085) ;
#13947 = AXIS2_PLACEMENT_3D('',#20390,#16086,#16087) ;
#13948 = AXIS2_PLACEMENT_3D('',#20391,#16088,#16089) ;
#13949 = AXIS2_PLACEMENT_3D('',#20393,#16090,#16091) ;
#13950 = AXIS2_PLACEMENT_3D('',#20396,#16093,#16094) ;
#13951 = AXIS2_PLACEMENT_3D('',#20397,#16095,#16096) ;
#13952 = AXIS2_PLACEMENT_3D('',#20398,#16097,#16098) ;
#13953 = AXIS2_PLACEMENT_3D('',#20400,#16099,#16100) ;
#13954 = AXIS2_PLACEMENT_3D('',#20403,#16102,#16103) ;
#13955 = AXIS2_PLACEMENT_3D('',#20404,#16104,#16105) ;
#13956 = AXIS2_PLACEMENT_3D('',#20405,#16106,#16107) ;
#13957 = AXIS2_PLACEMENT_3D('',#20407,#16108,#16109) ;
#13958 = AXIS2_PLACEMENT_3D('',#20410,#16111,#16112) ;
#13959 = AXIS2_PLACEMENT_3D('',#20411,#16113,#16114) ;
#13960 = AXIS2_PLACEMENT_3D('',#20412,#16115,#16116) ;
#13961 = AXIS2_PLACEMENT_3D('',#20414,#16117,#16118) ;
#13962 = AXIS2_PLACEMENT_3D('',#20417,#16120,#16121) ;
#13963 = AXIS2_PLACEMENT_3D('',#20418,#16122,#16123) ;
#13964 = AXIS2_PLACEMENT_3D('',#20419,#16124,#16125) ;
#13965 = AXIS2_PLACEMENT_3D('',#20421,#16126,#16127) ;
#13966 = AXIS2_PLACEMENT_3D('',#20424,#16129,#16130) ;
#13967 = AXIS2_PLACEMENT_3D('',#20425,#16131,#16132) ;
#13968 = AXIS2_PLACEMENT_3D('',#20426,#16133,#16134) ;
#13969 = AXIS2_PLACEMENT_3D('',#20428,#16135,#16136) ;
#13970 = AXIS2_PLACEMENT_3D('',#20431,#16138,#16139) ;
#13971 = AXIS2_PLACEMENT_3D('',#20432,#16140,#16141) ;
#13972 = AXIS2_PLACEMENT_3D('',#20433,#16142,#16143) ;
#13973 = AXIS2_PLACEMENT_3D('',#20435,#16144,#16145) ;
#13974 = AXIS2_PLACEMENT_3D('',#20438,#16147,#16148) ;
#13975 = AXIS2_PLACEMENT_3D('',#20439,#16149,#16150) ;
#13976 = AXIS2_PLACEMENT_3D('',#20441,#16151,#16152) ;
#13977 = AXIS2_PLACEMENT_3D('',#20444,#16154,#16155) ;
#13978 = AXIS2_PLACEMENT_3D('',#20445,#16156,#16157) ;
#13979 = AXIS2_PLACEMENT_3D('',#20447,#16158,#16159) ;
#13980 = AXIS2_PLACEMENT_3D('',#20450,#16161,#16162) ;
#13981 = AXIS2_PLACEMENT_3D('',#20451,#16163,#16164) ;
#13982 = AXIS2_PLACEMENT_3D('',#20453,#16165,#16166) ;
#13983 = AXIS2_PLACEMENT_3D('',#20456,#16168,#16169) ;
#13984 = AXIS2_PLACEMENT_3D('',#20457,#16170,#16171) ;
#13985 = AXIS2_PLACEMENT_3D('',#20459,#16172,#16173) ;
#13986 = AXIS2_PLACEMENT_3D('',#20462,#16175,#16176) ;
#13987 = AXIS2_PLACEMENT_3D('',#20463,#16177,#16178) ;
#13988 = AXIS2_PLACEMENT_3D('',#20465,#16179,#16180) ;
#13989 = AXIS2_PLACEMENT_3D('',#20468,#16182,#16183) ;
#13990 = AXIS2_PLACEMENT_3D('',#20469,#16184,#16185) ;
#13991 = AXIS2_PLACEMENT_3D('',#20471,#16186,#16187) ;
#13992 = AXIS2_PLACEMENT_3D('',#20474,#16189,#16190) ;
#13993 = AXIS2_PLACEMENT_3D('',#20475,#16191,#16192) ;
#13994 = AXIS2_PLACEMENT_3D('',#20477,#16193,#16194) ;
#13995 = AXIS2_PLACEMENT_3D('',#20480,#16196,#16197) ;
#13996 = AXIS2_PLACEMENT_3D('',#20481,#16198,#16199) ;
#13997 = AXIS2_PLACEMENT_3D('',#20483,#16200,#16201) ;
#13998 = AXIS2_PLACEMENT_3D('',#20486,#16203,#16204) ;
#13999 = AXIS2_PLACEMENT_3D('',#20487,#16205,#16206) ;
#14000 = AXIS2_PLACEMENT_3D('',#20489,#16207,#16208) ;
#14001 = AXIS2_PLACEMENT_3D('',#20492,#16210,#16211) ;
#14002 = AXIS2_PLACEMENT_3D('',#20493,#16212,#16213) ;
#14003 = AXIS2_PLACEMENT_3D('',#20495,#16214,#16215) ;
#14004 = AXIS2_PLACEMENT_3D('',#20498,#16217,#16218) ;
#14005 = AXIS2_PLACEMENT_3D('',#20499,#16219,#16220) ;
#14006 = AXIS2_PLACEMENT_3D('',#20501,#16221,#16222) ;
#14007 = AXIS2_PLACEMENT_3D('',#20504,#16224,#16225) ;
#14008 = AXIS2_PLACEMENT_3D('',#20505,#16226,#16227) ;
#14009 = AXIS2_PLACEMENT_3D('',#20507,#16228,#16229) ;
#14010 = AXIS2_PLACEMENT_3D('',#20510,#16231,#16232) ;
#14011 = AXIS2_PLACEMENT_3D('',#20511,#16233,#16234) ;
#14012 = AXIS2_PLACEMENT_3D('',#20513,#16235,#16236) ;
#14013 = AXIS2_PLACEMENT_3D('',#20516,#16238,#16239) ;
#14014 = AXIS2_PLACEMENT_3D('',#20517,#16240,#16241) ;
#14015 = AXIS2_PLACEMENT_3D('',#20519,#16242,#16243) ;
#14016 = AXIS2_PLACEMENT_3D('',#20522,#16245,#16246) ;
#14017 = AXIS2_PLACEMENT_3D('',#20523,#16247,#16248) ;
#14018 = AXIS2_PLACEMENT_3D('',#20525,#16249,#16250) ;
#14019 = AXIS2_PLACEMENT_3D('',#20528,#16252,#16253) ;
#14020 = AXIS2_PLACEMENT_3D('',#20529,#16254,#16255) ;
#14021 = AXIS2_PLACEMENT_3D('',#20531,#16256,#16257) ;
#14022 = AXIS2_PLACEMENT_3D('',#20534,#16259,#16260) ;
#14023 = AXIS2_PLACEMENT_3D('',#20535,#16261,#16262) ;
#14024 = AXIS2_PLACEMENT_3D('',#20537,#16263,#16264) ;
#14025 = AXIS2_PLACEMENT_3D('',#20540,#16266,#16267) ;
#14026 = AXIS2_PLACEMENT_3D('',#20541,#16268,#16269) ;
#14027 = AXIS2_PLACEMENT_3D('',#20543,#16270,#16271) ;
#14028 = AXIS2_PLACEMENT_3D('',#20546,#16273,#16274) ;
#14029 = AXIS2_PLACEMENT_3D('',#20547,#16275,#16276) ;
#14030 = AXIS2_PLACEMENT_3D('',#20549,#16277,#16278) ;
#14031 = AXIS2_PLACEMENT_3D('',#20552,#16280,#16281) ;
#14032 = AXIS2_PLACEMENT_3D('',#20553,#16282,#16283) ;
#14033 = AXIS2_PLACEMENT_3D('',#20555,#16284,#16285) ;
#14034 = AXIS2_PLACEMENT_3D('',#20558,#16287,#16288) ;
#14035 = AXIS2_PLACEMENT_3D('',#20559,#16289,#16290) ;
#14036 = AXIS2_PLACEMENT_3D('',#20561,#16291,#16292) ;
#14037 = AXIS2_PLACEMENT_3D('',#20564,#16294,#16295) ;
#14038 = AXIS2_PLACEMENT_3D('',#20565,#16296,#16297) ;
#14039 = AXIS2_PLACEMENT_3D('',#20567,#16298,#16299) ;
#14040 = AXIS2_PLACEMENT_3D('',#20570,#16301,#16302) ;
#14041 = AXIS2_PLACEMENT_3D('',#20571,#16303,#16304) ;
#14042 = AXIS2_PLACEMENT_3D('',#20573,#16305,#16306) ;
#14043 = AXIS2_PLACEMENT_3D('',#20576,#16308,#16309) ;
#14044 = AXIS2_PLACEMENT_3D('',#20577,#16310,#16311) ;
#14045 = AXIS2_PLACEMENT_3D('',#20579,#16312,#16313) ;
#14046 = AXIS2_PLACEMENT_3D('',#20582,#16315,#16316) ;
#14047 = AXIS2_PLACEMENT_3D('',#20583,#16317,#16318) ;
#14048 = AXIS2_PLACEMENT_3D('',#20585,#16319,#16320) ;
#14049 = AXIS2_PLACEMENT_3D('',#20588,#16322,#16323) ;
#14050 = AXIS2_PLACEMENT_3D('',#20589,#16324,#16325) ;
#14051 = AXIS2_PLACEMENT_3D('',#20591,#16326,#16327) ;
#14052 = AXIS2_PLACEMENT_3D('',#20594,#16329,#16330) ;
#14053 = AXIS2_PLACEMENT_3D('',#20595,#16331,#16332) ;
#14054 = AXIS2_PLACEMENT_3D('',#20597,#16333,#16334) ;
#14055 = AXIS2_PLACEMENT_3D('',#20600,#16336,#16337) ;
#14056 = AXIS2_PLACEMENT_3D('',#20601,#16338,#16339) ;
#14057 = AXIS2_PLACEMENT_3D('',#20603,#16340,#16341) ;
#14058 = AXIS2_PLACEMENT_3D('',#20606,#16343,#16344) ;
#14059 = AXIS2_PLACEMENT_3D('',#20607,#16345,#16346) ;
#14060 = AXIS2_PLACEMENT_3D('',#20608,#16347,#16348) ;
#14061 = AXIS2_PLACEMENT_3D('',#20609,#16349,#16350) ;
#14062 = AXIS2_PLACEMENT_3D('',#20610,#16351,#16352) ;
#14063 = AXIS2_PLACEMENT_3D('',#20612,#16353,#16354) ;
#14064 = AXIS2_PLACEMENT_3D('',#20614,#16355,#16356) ;
#14065 = AXIS2_PLACEMENT_3D('',#20615,#16357,#16358) ;
#14066 = AXIS2_PLACEMENT_3D('',#20617,#16359,#16360) ;
#14067 = AXIS2_PLACEMENT_3D('',#20619,#16361,#16362) ;
#14068 = AXIS2_PLACEMENT_3D('',#20620,#16363,#16364) ;
#14069 = AXIS2_PLACEMENT_3D('',#20622,#16366,#16367) ;
#14070 = AXIS2_PLACEMENT_3D('',#20624,#16369,#16370) ;
#14071 = AXIS2_PLACEMENT_3D('',#20626,#16371,#16372) ;
#14072 = AXIS2_PLACEMENT_3D('',#20628,#16373,#16374) ;
#14073 = AXIS2_PLACEMENT_3D('',#20629,#16375,#16376) ;
#14074 = AXIS2_PLACEMENT_3D('',#20631,#16377,#16378) ;
#14075 = AXIS2_PLACEMENT_3D('',#20633,#16380,#16381) ;
#14076 = AXIS2_PLACEMENT_3D('',#20635,#16382,#16383) ;
#14077 = AXIS2_PLACEMENT_3D('',#20636,#16384,#16385) ;
#14078 = AXIS2_PLACEMENT_3D('',#20638,#16387,#16388) ;
#14079 = AXIS2_PLACEMENT_3D('',#20639,#16389,#16390) ;
#14080 = AXIS2_PLACEMENT_3D('',#20641,#16391,#16392) ;
#14081 = AXIS2_PLACEMENT_3D('',#20643,#16393,#16394) ;
#14082 = AXIS2_PLACEMENT_3D('',#20644,#16395,#16396) ;
#14083 = AXIS2_PLACEMENT_3D('',#20646,#16397,#16398) ;
#14084 = AXIS2_PLACEMENT_3D('',#20648,#16399,#16400) ;
#14085 = AXIS2_PLACEMENT_3D('',#20649,#16401,#16402) ;
#14086 = AXIS2_PLACEMENT_3D('',#20651,#16404,#16405) ;
#14087 = AXIS2_PLACEMENT_3D('',#20653,#16407,#16408) ;
#14088 = AXIS2_PLACEMENT_3D('',#20655,#16409,#16410) ;
#14089 = AXIS2_PLACEMENT_3D('',#20657,#16411,#16412) ;
#14090 = AXIS2_PLACEMENT_3D('',#20658,#16413,#16414) ;
#14091 = AXIS2_PLACEMENT_3D('',#20660,#16415,#16416) ;
#14092 = AXIS2_PLACEMENT_3D('',#20662,#16418,#16419) ;
#14093 = AXIS2_PLACEMENT_3D('',#20664,#16420,#16421) ;
#14094 = AXIS2_PLACEMENT_3D('',#20665,#16422,#16423) ;
#14095 = AXIS2_PLACEMENT_3D('',#20667,#16425,#16426) ;
#14096 = AXIS2_PLACEMENT_3D('',#20668,#16427,#16428) ;
#14097 = AXIS2_PLACEMENT_3D('',#20670,#16429,#16430) ;
#14098 = AXIS2_PLACEMENT_3D('',#20673,#16432,#16433) ;
#14099 = AXIS2_PLACEMENT_3D('',#20674,#16434,#16435) ;
#14100 = AXIS2_PLACEMENT_3D('',#20676,#16436,#16437) ;
#14101 = AXIS2_PLACEMENT_3D('',#20679,#16439,#16440) ;
#14102 = AXIS2_PLACEMENT_3D('',#20680,#16441,#16442) ;
#14103 = AXIS2_PLACEMENT_3D('',#20681,#16443,#16444) ;
#14104 = AXIS2_PLACEMENT_3D('',#20682,#16445,#16446) ;
#14105 = AXIS2_PLACEMENT_3D('',#20683,#16447,#16448) ;
#14106 = AXIS2_PLACEMENT_3D('',#20692,#16453,#16454) ;
#14107 = AXIS2_PLACEMENT_3D('',#20701,#16459,#16460) ;
#14108 = AXIS2_PLACEMENT_3D('',#20702,#16461,#16462) ;
#14109 = AXIS2_PLACEMENT_3D('',#20703,#16463,#16464) ;
#14110 = AXIS2_PLACEMENT_3D('',#20704,#16465,#16466) ;
#14111 = AXIS2_PLACEMENT_3D('',#20705,#16467,#16468) ;
#14112 = AXIS2_PLACEMENT_3D('',#20706,#16469,#16470) ;
#14113 = AXIS2_PLACEMENT_3D('',#20707,#16471,#16472) ;
#14114 = AXIS2_PLACEMENT_3D('',#20708,#16473,#16474) ;
#14115 = AXIS2_PLACEMENT_3D('',#20709,#16475,#16476) ;
#14116 = AXIS2_PLACEMENT_3D('',#20710,#16477,#16478) ;
#14117 = AXIS2_PLACEMENT_3D('',#20719,#16483,#16484) ;
#14118 = AXIS2_PLACEMENT_3D('',#20728,#16489,#16490) ;
#14119 = AXIS2_PLACEMENT_3D('',#20731,#16493,#16494) ;
#14120 = AXIS2_PLACEMENT_3D('',#20733,#16495,#16496) ;
#14121 = AXIS2_PLACEMENT_3D('',#20734,#16497,#16498) ;
#14122 = AXIS2_PLACEMENT_3D('',#20735,#16499,#16500) ;
#14123 = AXIS2_PLACEMENT_3D('',#20736,#16501,#16502) ;
#14124 = AXIS2_PLACEMENT_3D('',#20737,#16503,#16504) ;
#14125 = AXIS2_PLACEMENT_3D('',#20746,#16509,#16510) ;
#14126 = AXIS2_PLACEMENT_3D('',#20755,#16515,#16516) ;
#14127 = AXIS2_PLACEMENT_3D('',#20758,#16519,#16520) ;
#14128 = AXIS2_PLACEMENT_3D('',#20760,#16521,#16522) ;
#14129 = AXIS2_PLACEMENT_3D('',#20763,#16524,#16525) ;
#14130 = AXIS2_PLACEMENT_3D('',#20764,#16526,#16527) ;
#14131 = AXIS2_PLACEMENT_3D('',#20766,#16528,#16529) ;
#14132 = AXIS2_PLACEMENT_3D('',#20769,#16531,#16532) ;
#14133 = AXIS2_PLACEMENT_3D('',#20770,#16533,#16534) ;
#14134 = AXIS2_PLACEMENT_3D('',#20778,#16538,#16539) ;
#14135 = AXIS2_PLACEMENT_3D('',#20786,#16543,#16544) ;
#14136 = AXIS2_PLACEMENT_3D('',#20794,#16548,#16549) ;
#14137 = AXIS2_PLACEMENT_3D('',#20802,#16553,#16554) ;
#14138 = AXIS2_PLACEMENT_3D('',#20810,#16558,#16559) ;
#14139 = AXIS2_PLACEMENT_3D('',#20818,#16563,#16564) ;
#14140 = AXIS2_PLACEMENT_3D('',#20826,#16568,#16569) ;
#14141 = AXIS2_PLACEMENT_3D('',#20834,#16573,#16574) ;
#14142 = AXIS2_PLACEMENT_3D('',#20842,#16578,#16579) ;
#14143 = AXIS2_PLACEMENT_3D('',#20850,#16583,#16584) ;
#14144 = AXIS2_PLACEMENT_3D('',#20856,#16588,#16589) ;
#14145 = AXIS2_PLACEMENT_3D('',#20860,#16592,#16593) ;
#14146 = AXIS2_PLACEMENT_3D('',#20866,#16597,#16598) ;
#14147 = AXIS2_PLACEMENT_3D('',#20868,#16600,#16601) ;
#14148 = AXIS2_PLACEMENT_3D('',#20870,#16602,#16603) ;
#14149 = AXIS2_PLACEMENT_3D('',#20872,#16605,#16606) ;
#14150 = AXIS2_PLACEMENT_3D('',#20878,#16610,#16611) ;
#14151 = AXIS2_PLACEMENT_3D('',#20882,#16614,#16615) ;
#14152 = AXIS2_PLACEMENT_3D('',#20884,#16617,#16618) ;
#14153 = AXIS2_PLACEMENT_3D('',#20886,#16619,#16620) ;
#14154 = AXIS2_PLACEMENT_3D('',#20888,#16622,#16623) ;
#14155 = AXIS2_PLACEMENT_3D('',#20892,#16626,#16627) ;
#14156 = AXIS2_PLACEMENT_3D('',#20898,#16631,#16632) ;
#14157 = AXIS2_PLACEMENT_3D('',#20900,#16634,#16635) ;
#14158 = AXIS2_PLACEMENT_3D('',#20902,#16636,#16637) ;
#14159 = AXIS2_PLACEMENT_3D('',#20904,#16639,#16640) ;
#14160 = AXIS2_PLACEMENT_3D('',#20910,#16644,#16645) ;
#14161 = AXIS2_PLACEMENT_3D('',#20914,#16648,#16649) ;
#14162 = AXIS2_PLACEMENT_3D('',#20916,#16651,#16652) ;
#14163 = AXIS2_PLACEMENT_3D('',#20918,#16653,#16654) ;
#14164 = AXIS2_PLACEMENT_3D('',#20920,#16656,#16657) ;
#14165 = AXIS2_PLACEMENT_3D('',#20924,#16660,#16661) ;
#14166 = AXIS2_PLACEMENT_3D('',#20930,#16665,#16666) ;
#14167 = AXIS2_PLACEMENT_3D('',#20932,#16668,#16669) ;
#14168 = AXIS2_PLACEMENT_3D('',#20934,#16670,#16671) ;
#14169 = AXIS2_PLACEMENT_3D('',#20936,#16673,#16674) ;
#14170 = AXIS2_PLACEMENT_3D('',#20942,#16678,#16679) ;
#14171 = AXIS2_PLACEMENT_3D('',#20946,#16682,#16683) ;
#14172 = AXIS2_PLACEMENT_3D('',#20948,#16685,#16686) ;
#14173 = AXIS2_PLACEMENT_3D('',#20950,#16687,#16688) ;
#14174 = AXIS2_PLACEMENT_3D('',#20952,#16690,#16691) ;
#14175 = AXIS2_PLACEMENT_3D('',#20956,#16694,#16695) ;
#14176 = AXIS2_PLACEMENT_3D('',#20962,#16699,#16700) ;
#14177 = AXIS2_PLACEMENT_3D('',#20964,#16702,#16703) ;
#14178 = AXIS2_PLACEMENT_3D('',#20966,#16704,#16705) ;
#14179 = AXIS2_PLACEMENT_3D('',#20968,#16707,#16708) ;
#14180 = AXIS2_PLACEMENT_3D('',#20974,#16712,#16713) ;
#14181 = AXIS2_PLACEMENT_3D('',#20978,#16716,#16717) ;
#14182 = AXIS2_PLACEMENT_3D('',#20980,#16719,#16720) ;
#14183 = AXIS2_PLACEMENT_3D('',#20982,#16721,#16722) ;
#14184 = AXIS2_PLACEMENT_3D('',#20984,#16724,#16725) ;
#14185 = AXIS2_PLACEMENT_3D('',#20988,#16728,#16729) ;
#14186 = AXIS2_PLACEMENT_3D('',#20994,#16733,#16734) ;
#14187 = AXIS2_PLACEMENT_3D('',#20996,#16736,#16737) ;
#14188 = AXIS2_PLACEMENT_3D('',#20998,#16738,#16739) ;
#14189 = AXIS2_PLACEMENT_3D('',#21000,#16741,#16742) ;
#14190 = AXIS2_PLACEMENT_3D('',#21006,#16746,#16747) ;
#14191 = AXIS2_PLACEMENT_3D('',#21010,#16750,#16751) ;
#14192 = AXIS2_PLACEMENT_3D('',#21012,#16753,#16754) ;
#14193 = AXIS2_PLACEMENT_3D('',#21014,#16755,#16756) ;
#14194 = AXIS2_PLACEMENT_3D('',#21016,#16758,#16759) ;
#14195 = AXIS2_PLACEMENT_3D('',#21020,#16762,#16763) ;
#14196 = AXIS2_PLACEMENT_3D('',#21024,#16766,#16767) ;
#14197 = AXIS2_PLACEMENT_3D('',#21026,#16769,#16770) ;
#14198 = AXIS2_PLACEMENT_3D('',#21028,#16771,#16772) ;
#14199 = AXIS2_PLACEMENT_3D('',#21030,#16774,#16775) ;
#14200 = AXIS2_PLACEMENT_3D('',#21031,#16776,#16777) ;
#14201 = AXIS2_PLACEMENT_3D('',#21032,#16778,#16779) ;
#14202 = AXIS2_PLACEMENT_3D('',#21041,#16784,#16785) ;
#14203 = AXIS2_PLACEMENT_3D('',#21050,#16790,#16791) ;
#14204 = AXIS2_PLACEMENT_3D('',#21053,#16794,#16795) ;
#14205 = AXIS2_PLACEMENT_3D('',#21055,#16797,#16798) ;
#14206 = AXIS2_PLACEMENT_3D('',#21057,#16800,#16801) ;
#14207 = AXIS2_PLACEMENT_3D('',#21058,#16802,#16803) ;
#14208 = AXIS2_PLACEMENT_3D('',#21059,#16804,#16805) ;
#14209 = AXIS2_PLACEMENT_3D('',#21061,#16806,#16807) ;
#14210 = AXIS2_PLACEMENT_3D('',#21064,#16809,#16810) ;
#14211 = AXIS2_PLACEMENT_3D('',#21065,#16811,#16812) ;
#14212 = AXIS2_PLACEMENT_3D('',#21067,#16813,#16814) ;
#14213 = AXIS2_PLACEMENT_3D('',#21070,#16816,#16817) ;
#14214 = AXIS2_PLACEMENT_3D('',#21071,#16818,#16819) ;
#14215 = AXIS2_PLACEMENT_3D('',#21072,#16820,#16821) ;
#14216 = AXIS2_PLACEMENT_3D('',#21073,#16822,#16823) ;
#14217 = AXIS2_PLACEMENT_3D('',#21074,#16824,#16825) ;
#14218 = AXIS2_PLACEMENT_3D('',#21083,#16830,#16831) ;
#14219 = AXIS2_PLACEMENT_3D('',#21089,#16835,#16836) ;
#14220 = AXIS2_PLACEMENT_3D('',#21093,#16839,#16840) ;
#14221 = AXIS2_PLACEMENT_3D('',#21097,#16843,#16844) ;
#14222 = AXIS2_PLACEMENT_3D('',#21107,#16850,#16851) ;
#14223 = AXIS2_PLACEMENT_3D('',#21113,#16855,#16856) ;
#14224 = AXIS2_PLACEMENT_3D('',#21119,#16860,#16861) ;
#14225 = AXIS2_PLACEMENT_3D('',#21122,#16864,#16865) ;
#14226 = AXIS2_PLACEMENT_3D('',#21123,#16866,#16867) ;
#14227 = AXIS2_PLACEMENT_3D('',#21124,#16868,#16869) ;
#14228 = AXIS2_PLACEMENT_3D('',#21125,#16870,#16871) ;
#14229 = AXIS2_PLACEMENT_3D('',#21127,#16872,#16873) ;
#14230 = AXIS2_PLACEMENT_3D('',#21130,#16875,#16876) ;
#14231 = AXIS2_PLACEMENT_3D('',#21131,#16877,#16878) ;
#14232 = AXIS2_PLACEMENT_3D('',#21132,#16879,#16880) ;
#14233 = AXIS2_PLACEMENT_3D('',#21134,#16881,#16882) ;
#14234 = AXIS2_PLACEMENT_3D('',#21137,#16884,#16885) ;
#14235 = AXIS2_PLACEMENT_3D('',#21138,#16886,#16887) ;
#14236 = AXIS2_PLACEMENT_3D('',#21143,#16889,#16890) ;
#14237 = AXIS2_PLACEMENT_3D('',#21146,#16892,#16893) ;
#14238 = AXIS2_PLACEMENT_3D('',#21147,#16894,#16895) ;
#14239 = AXIS2_PLACEMENT_3D('',#21152,#16897,#16898) ;
#14240 = AXIS2_PLACEMENT_3D('',#21155,#16900,#16901) ;
#14241 = AXIS2_PLACEMENT_3D('',#21156,#16902,#16903) ;
#14242 = AXIS2_PLACEMENT_3D('',#21161,#16905,#16906) ;
#14243 = AXIS2_PLACEMENT_3D('',#21164,#16908,#16909) ;
#14244 = AXIS2_PLACEMENT_3D('',#21165,#16910,#16911) ;
#14245 = AXIS2_PLACEMENT_3D('',#21171,#16915,#16916) ;
#14246 = AXIS2_PLACEMENT_3D('',#21177,#16920,#16921) ;
#14247 = AXIS2_PLACEMENT_3D('',#21183,#16925,#16926) ;
#14248 = AXIS2_PLACEMENT_3D('',#21189,#16931,#16932) ;
#14249 = AXIS2_PLACEMENT_3D('',#21191,#16934,#16935) ;
#14250 = AXIS2_PLACEMENT_3D('',#21195,#16938,#16939) ;
#14251 = AXIS2_PLACEMENT_3D('',#21198,#16942,#16943) ;
#14252 = AXIS2_PLACEMENT_3D('',#21199,#16944,#16945) ;
#14253 = AXIS2_PLACEMENT_3D('',#21200,#16946,#16947) ;
#14254 = AXIS2_PLACEMENT_3D('',#21201,#16948,#16949) ;
#14255 = AXIS2_PLACEMENT_3D('',#21203,#16950,#16951) ;
#14256 = AXIS2_PLACEMENT_3D('',#21206,#16953,#16954) ;
#14257 = AXIS2_PLACEMENT_3D('',#21207,#16955,#16956) ;
#14258 = AXIS2_PLACEMENT_3D('',#21208,#16957,#16958) ;
#14259 = AXIS2_PLACEMENT_3D('',#21209,#16959,#16960) ;
#14260 = AXIS2_PLACEMENT_3D('',#21210,#16961,#16962) ;
#14261 = AXIS2_PLACEMENT_3D('',#21213,#16963,#16964) ;
#14262 = AXIS2_PLACEMENT_3D('',#21214,#16965,#16966) ;
#14263 = AXIS2_PLACEMENT_3D('',#21215,#16967,#16968) ;
#14264 = AXIS2_PLACEMENT_3D('',#21218,#16969,#16970) ;
#14265 = AXIS2_PLACEMENT_3D('',#21220,#16971,#16972) ;
#14266 = AXIS2_PLACEMENT_3D('',#21222,#16973,#16974) ;
#14267 = AXIS2_PLACEMENT_3D('',#21224,#16975,#16976) ;
#14268 = AXIS2_PLACEMENT_3D('',#21225,#16977,#16978) ;
#14269 = AXIS2_PLACEMENT_3D('',#21226,#16979,#16980) ;
#14270 = AXIS2_PLACEMENT_3D('',#21229,#16981,#16982) ;
#14271 = AXIS2_PLACEMENT_3D('',#21231,#16983,#16984) ;
#14272 = AXIS2_PLACEMENT_3D('',#21233,#16985,#16986) ;
#14273 = AXIS2_PLACEMENT_3D('',#21234,#16987,#16988) ;
#14274 = AXIS2_PLACEMENT_3D('',#21235,#16989,#16990) ;
#14275 = AXIS2_PLACEMENT_3D('',#21238,#16991,#16992) ;
#14276 = AXIS2_PLACEMENT_3D('',#21240,#16993,#16994) ;
#14277 = AXIS2_PLACEMENT_3D('',#21242,#16995,#16996) ;
#14278 = AXIS2_PLACEMENT_3D('',#21243,#16997,#16998) ;
#14279 = AXIS2_PLACEMENT_3D('',#21244,#16999,#17000) ;
#14280 = AXIS2_PLACEMENT_3D('',#21247,#17001,#17002) ;
#14281 = AXIS2_PLACEMENT_3D('',#21249,#17003,#17004) ;
#14282 = AXIS2_PLACEMENT_3D('',#21251,#17005,#17006) ;
#14283 = AXIS2_PLACEMENT_3D('',#21252,#17007,#17008) ;
#14284 = AXIS2_PLACEMENT_3D('',#21253,#17009,#17010) ;
#14285 = AXIS2_PLACEMENT_3D('',#21256,#17011,#17012) ;
#14286 = AXIS2_PLACEMENT_3D('',#21258,#17013,#17014) ;
#14287 = AXIS2_PLACEMENT_3D('',#21260,#17015,#17016) ;
#14288 = AXIS2_PLACEMENT_3D('',#21262,#17017,#17018) ;
#14289 = AXIS2_PLACEMENT_3D('',#21263,#17019,#17020) ;
#14290 = AXIS2_PLACEMENT_3D('',#21264,#17021,#17022) ;
#14291 = AXIS2_PLACEMENT_3D('',#21267,#17023,#17024) ;
#14292 = AXIS2_PLACEMENT_3D('',#21268,#17025,#17026) ;
#14293 = AXIS2_PLACEMENT_3D('',#21269,#17027,#17028) ;
#14294 = AXIS2_PLACEMENT_3D('',#21272,#17029,#17030) ;
#14295 = AXIS2_PLACEMENT_3D('',#21273,#17031,#17032) ;
#14296 = AXIS2_PLACEMENT_3D('',#21274,#17033,#17034) ;
#14297 = AXIS2_PLACEMENT_3D('',#21277,#17035,#17036) ;
#14298 = AXIS2_PLACEMENT_3D('',#21278,#17037,#17038) ;
#14299 = AXIS2_PLACEMENT_3D('',#21279,#17039,#17040) ;
#14300 = AXIS2_PLACEMENT_3D('',#21282,#17041,#17042) ;
#14301 = AXIS2_PLACEMENT_3D('',#21284,#17043,#17044) ;
#14302 = AXIS2_PLACEMENT_3D('',#21286,#17045,#17046) ;
#14303 = AXIS2_PLACEMENT_3D('',#21288,#17047,#17048) ;
#14304 = AXIS2_PLACEMENT_3D('',#21289,#17049,#17050) ;
#14305 = AXIS2_PLACEMENT_3D('',#21290,#17051,#17052) ;
#14306 = AXIS2_PLACEMENT_3D('',#21293,#17053,#17054) ;
#14307 = AXIS2_PLACEMENT_3D('',#21295,#17055,#17056) ;
#14308 = AXIS2_PLACEMENT_3D('',#21297,#17057,#17058) ;
#14309 = AXIS2_PLACEMENT_3D('',#21298,#17059,#17060) ;
#14310 = AXIS2_PLACEMENT_3D('',#21299,#17061,#17062) ;
#14311 = AXIS2_PLACEMENT_3D('',#21302,#17063,#17064) ;
#14312 = AXIS2_PLACEMENT_3D('',#21304,#17065,#17066) ;
#14313 = AXIS2_PLACEMENT_3D('',#21306,#17067,#17068) ;
#14314 = AXIS2_PLACEMENT_3D('',#21307,#17069,#17070) ;
#14315 = AXIS2_PLACEMENT_3D('',#21308,#17071,#17072) ;
#14316 = AXIS2_PLACEMENT_3D('',#21311,#17073,#17074) ;
#14317 = AXIS2_PLACEMENT_3D('',#21313,#17075,#17076) ;
#14318 = AXIS2_PLACEMENT_3D('',#21315,#17077,#17078) ;
#14319 = AXIS2_PLACEMENT_3D('',#21316,#17079,#17080) ;
#14320 = AXIS2_PLACEMENT_3D('',#21317,#17081,#17082) ;
#14321 = AXIS2_PLACEMENT_3D('',#21320,#17083,#17084) ;
#14322 = AXIS2_PLACEMENT_3D('',#21322,#17085,#17086) ;
#14323 = AXIS2_PLACEMENT_3D('',#21324,#17087,#17088) ;
#14324 = AXIS2_PLACEMENT_3D('',#21326,#17089,#17090) ;
#14325 = AXIS2_PLACEMENT_3D('',#21327,#17091,#17092) ;
#14326 = AXIS2_PLACEMENT_3D('',#21328,#17093,#17094) ;
#14327 = AXIS2_PLACEMENT_3D('',#21331,#17095,#17096) ;
#14328 = AXIS2_PLACEMENT_3D('',#21332,#17097,#17098) ;
#14329 = AXIS2_PLACEMENT_3D('',#21333,#17099,#17100) ;
#14330 = AXIS2_PLACEMENT_3D('',#21336,#17101,#17102) ;
#14331 = AXIS2_PLACEMENT_3D('',#21337,#17103,#17104) ;
#14332 = AXIS2_PLACEMENT_3D('',#21338,#17105,#17106) ;
#14333 = AXIS2_PLACEMENT_3D('',#21341,#17107,#17108) ;
#14334 = AXIS2_PLACEMENT_3D('',#21342,#17109,#17110) ;
#14335 = AXIS2_PLACEMENT_3D('',#21343,#17111,#17112) ;
#14336 = AXIS2_PLACEMENT_3D('',#21346,#17113,#17114) ;
#14337 = AXIS2_PLACEMENT_3D('',#21348,#17115,#17116) ;
#14338 = AXIS2_PLACEMENT_3D('',#21350,#17117,#17118) ;
#14339 = AXIS2_PLACEMENT_3D('',#21352,#17119,#17120) ;
#14340 = AXIS2_PLACEMENT_3D('',#21353,#17121,#17122) ;
#14341 = AXIS2_PLACEMENT_3D('',#21354,#17123,#17124) ;
#14342 = AXIS2_PLACEMENT_3D('',#21357,#17125,#17126) ;
#14343 = AXIS2_PLACEMENT_3D('',#21359,#17127,#17128) ;
#14344 = AXIS2_PLACEMENT_3D('',#21361,#17129,#17130) ;
#14345 = AXIS2_PLACEMENT_3D('',#21362,#17131,#17132) ;
#14346 = AXIS2_PLACEMENT_3D('',#21363,#17133,#17134) ;
#14347 = AXIS2_PLACEMENT_3D('',#21366,#17135,#17136) ;
#14348 = AXIS2_PLACEMENT_3D('',#21368,#17137,#17138) ;
#14349 = AXIS2_PLACEMENT_3D('',#21370,#17139,#17140) ;
#14350 = AXIS2_PLACEMENT_3D('',#21371,#17141,#17142) ;
#14351 = AXIS2_PLACEMENT_3D('',#21372,#17143,#17144) ;
#14352 = AXIS2_PLACEMENT_3D('',#21375,#17145,#17146) ;
#14353 = AXIS2_PLACEMENT_3D('',#21377,#17147,#17148) ;
#14354 = AXIS2_PLACEMENT_3D('',#21379,#17149,#17150) ;
#14355 = AXIS2_PLACEMENT_3D('',#21380,#17151,#17152) ;
#14356 = AXIS2_PLACEMENT_3D('',#21381,#17153,#17154) ;
#14357 = AXIS2_PLACEMENT_3D('',#21384,#17155,#17156) ;
#14358 = AXIS2_PLACEMENT_3D('',#21386,#17157,#17158) ;
#14359 = AXIS2_PLACEMENT_3D('',#21388,#17159,#17160) ;
#14360 = AXIS2_PLACEMENT_3D('',#21390,#17161,#17162) ;
#14361 = AXIS2_PLACEMENT_3D('',#21391,#17163,#17164) ;
#14362 = AXIS2_PLACEMENT_3D('',#21392,#17165,#17166) ;
#14363 = AXIS2_PLACEMENT_3D('',#21395,#17167,#17168) ;
#14364 = AXIS2_PLACEMENT_3D('',#21396,#17169,#17170) ;
#14365 = AXIS2_PLACEMENT_3D('',#21397,#17171,#17172) ;
#14366 = AXIS2_PLACEMENT_3D('',#21400,#17173,#17174) ;
#14367 = AXIS2_PLACEMENT_3D('',#21401,#17175,#17176) ;
#14368 = AXIS2_PLACEMENT_3D('',#21402,#17177,#17178) ;
#14369 = AXIS2_PLACEMENT_3D('',#21405,#17179,#17180) ;
#14370 = AXIS2_PLACEMENT_3D('',#21406,#17181,#17182) ;
#14371 = AXIS2_PLACEMENT_3D('',#21407,#17183,#17184) ;
#14372 = AXIS2_PLACEMENT_3D('',#21410,#17185,#17186) ;
#14373 = AXIS2_PLACEMENT_3D('',#21412,#17187,#17188) ;
#14374 = AXIS2_PLACEMENT_3D('',#21414,#17189,#17190) ;
#14375 = AXIS2_PLACEMENT_3D('',#21416,#17191,#17192) ;
#14376 = AXIS2_PLACEMENT_3D('',#21417,#17193,#17194) ;
#14377 = AXIS2_PLACEMENT_3D('',#21418,#17195,#17196) ;
#14378 = AXIS2_PLACEMENT_3D('',#21421,#17197,#17198) ;
#14379 = AXIS2_PLACEMENT_3D('',#21423,#17199,#17200) ;
#14380 = AXIS2_PLACEMENT_3D('',#21425,#17201,#17202) ;
#14381 = AXIS2_PLACEMENT_3D('',#21426,#17203,#17204) ;
#14382 = AXIS2_PLACEMENT_3D('',#21427,#17205,#17206) ;
#14383 = AXIS2_PLACEMENT_3D('',#21430,#17207,#17208) ;
#14384 = AXIS2_PLACEMENT_3D('',#21432,#17209,#17210) ;
#14385 = AXIS2_PLACEMENT_3D('',#21434,#17211,#17212) ;
#14386 = AXIS2_PLACEMENT_3D('',#21435,#17213,#17214) ;
#14387 = AXIS2_PLACEMENT_3D('',#21436,#17215,#17216) ;
#14388 = AXIS2_PLACEMENT_3D('',#21439,#17217,#17218) ;
#14389 = AXIS2_PLACEMENT_3D('',#21441,#17219,#17220) ;
#14390 = AXIS2_PLACEMENT_3D('',#21443,#17221,#17222) ;
#14391 = AXIS2_PLACEMENT_3D('',#21444,#17223,#17224) ;
#14392 = AXIS2_PLACEMENT_3D('',#21445,#17225,#17226) ;
#14393 = AXIS2_PLACEMENT_3D('',#21448,#17227,#17228) ;
#14394 = AXIS2_PLACEMENT_3D('',#21450,#17229,#17230) ;
#14395 = AXIS2_PLACEMENT_3D('',#21452,#17231,#17232) ;
#14396 = AXIS2_PLACEMENT_3D('',#21454,#17233,#17234) ;
#14397 = AXIS2_PLACEMENT_3D('',#21455,#17235,#17236) ;
#14398 = AXIS2_PLACEMENT_3D('',#21456,#17237,#17238) ;
#14399 = AXIS2_PLACEMENT_3D('',#21459,#17239,#17240) ;
#14400 = AXIS2_PLACEMENT_3D('',#21460,#17241,#17242) ;
#14401 = AXIS2_PLACEMENT_3D('',#21461,#17243,#17244) ;
#14402 = AXIS2_PLACEMENT_3D('',#21463,#17245,#17246) ;
#14403 = AXIS2_PLACEMENT_3D('',#21467,#17248,#17249) ;
#14404 = AXIS2_PLACEMENT_3D('',#21468,#17250,#17251) ;
#14405 = AXIS2_PLACEMENT_3D('',#21469,#17252,#17253) ;
#14406 = AXIS2_PLACEMENT_3D('',#21470,#17254,#17255) ;
#14407 = AXIS2_PLACEMENT_3D('',#21471,#17256,#17257) ;
#14408 = AXIS2_PLACEMENT_3D('',#21474,#17259,#17260) ;
#14409 = AXIS2_PLACEMENT_3D('',#21475,#17261,#17262) ;
#14410 = AXIS2_PLACEMENT_3D('',#21476,#17263,#17264) ;
#14411 = AXIS2_PLACEMENT_3D('',#21478,#17266,#17267) ;
#14412 = AXIS2_PLACEMENT_3D('',#21479,#17268,#17269) ;
#14413 = AXIS2_PLACEMENT_3D('',#21481,#17271,#17272) ;
#14414 = AXIS2_PLACEMENT_3D('',#21482,#17273,#17274) ;
#14415 = AXIS2_PLACEMENT_3D('',#21484,#17276,#17277) ;
#14416 = AXIS2_PLACEMENT_3D('',#21485,#17278,#17279) ;
#14417 = AXIS2_PLACEMENT_3D('',#21488,#17281,#17282) ;
#14418 = AXIS2_PLACEMENT_3D('',#21489,#17283,#17284) ;
#14419 = AXIS2_PLACEMENT_3D('',#21490,#17285,#17286) ;
#14420 = AXIS2_PLACEMENT_3D('',#21494,#17288,#17289) ;
#14421 = AXIS2_PLACEMENT_3D('',#21495,#17290,#17291) ;
#14422 = AXIS2_PLACEMENT_3D('',#21496,#17292,#17293) ;
#14423 = AXIS2_PLACEMENT_3D('',#21497,#17294,#17295) ;
#14424 = AXIS2_PLACEMENT_3D('',#21500,#17297,#17298) ;
#14425 = AXIS2_PLACEMENT_3D('',#21501,#17299,#17300) ;
#14426 = AXIS2_PLACEMENT_3D('',#21502,#17301,#17302) ;
#14427 = AXIS2_PLACEMENT_3D('',#21506,#17304,#17305) ;
#14428 = AXIS2_PLACEMENT_3D('',#21507,#17306,#17307) ;
#14429 = AXIS2_PLACEMENT_3D('',#21508,#17308,#17309) ;
#14430 = AXIS2_PLACEMENT_3D('',#21509,#17310,#17311) ;
#14431 = AXIS2_PLACEMENT_3D('',#21512,#17313,#17314) ;
#14432 = AXIS2_PLACEMENT_3D('',#21513,#17315,#17316) ;
#14433 = AXIS2_PLACEMENT_3D('',#21514,#17317,#17318) ;
#14434 = AXIS2_PLACEMENT_3D('',#21516,#17320,#17321) ;
#14435 = AXIS2_PLACEMENT_3D('',#21517,#17322,#17323) ;
#14436 = AXIS2_PLACEMENT_3D('',#21519,#17325,#17326) ;
#14437 = AXIS2_PLACEMENT_3D('',#21520,#17327,#17328) ;
#14438 = AXIS2_PLACEMENT_3D('',#21522,#17330,#17331) ;
#14439 = AXIS2_PLACEMENT_3D('',#21523,#17332,#17333) ;
#14440 = AXIS2_PLACEMENT_3D('',#21526,#17335,#17336) ;
#14441 = AXIS2_PLACEMENT_3D('',#21527,#17337,#17338) ;
#14442 = AXIS2_PLACEMENT_3D('',#21528,#17339,#17340) ;
#14443 = AXIS2_PLACEMENT_3D('',#21532,#17342,#17343) ;
#14444 = AXIS2_PLACEMENT_3D('',#21533,#17344,#17345) ;
#14445 = AXIS2_PLACEMENT_3D('',#21534,#17346,#17347) ;
#14446 = AXIS2_PLACEMENT_3D('',#21535,#17348,#17349) ;
#14447 = AXIS2_PLACEMENT_3D('',#21538,#17351,#17352) ;
#14448 = AXIS2_PLACEMENT_3D('',#21539,#17353,#17354) ;
#14449 = AXIS2_PLACEMENT_3D('',#21540,#17355,#17356) ;
#14450 = AXIS2_PLACEMENT_3D('',#21544,#17358,#17359) ;
#14451 = AXIS2_PLACEMENT_3D('',#21545,#17360,#17361) ;
#14452 = AXIS2_PLACEMENT_3D('',#21546,#17362,#17363) ;
#14453 = AXIS2_PLACEMENT_3D('',#21547,#17364,#17365) ;
#14454 = AXIS2_PLACEMENT_3D('',#21550,#17367,#17368) ;
#14455 = AXIS2_PLACEMENT_3D('',#21551,#17369,#17370) ;
#14456 = AXIS2_PLACEMENT_3D('',#21552,#17371,#17372) ;
#14457 = AXIS2_PLACEMENT_3D('',#21554,#17374,#17375) ;
#14458 = AXIS2_PLACEMENT_3D('',#21555,#17376,#17377) ;
#14459 = AXIS2_PLACEMENT_3D('',#21557,#17379,#17380) ;
#14460 = AXIS2_PLACEMENT_3D('',#21558,#17381,#17382) ;
#14461 = AXIS2_PLACEMENT_3D('',#21560,#17384,#17385) ;
#14462 = AXIS2_PLACEMENT_3D('',#21561,#17386,#17387) ;
#14463 = AXIS2_PLACEMENT_3D('',#21564,#17389,#17390) ;
#14464 = AXIS2_PLACEMENT_3D('',#21565,#17391,#17392) ;
#14465 = AXIS2_PLACEMENT_3D('',#21566,#17393,#17394) ;
#14466 = AXIS2_PLACEMENT_3D('',#21570,#17396,#17397) ;
#14467 = AXIS2_PLACEMENT_3D('',#21571,#17398,#17399) ;
#14468 = AXIS2_PLACEMENT_3D('',#21572,#17400,#17401) ;
#14469 = AXIS2_PLACEMENT_3D('',#21573,#17402,#17403) ;
#14470 = AXIS2_PLACEMENT_3D('',#21576,#17405,#17406) ;
#14471 = AXIS2_PLACEMENT_3D('',#21577,#17407,#17408) ;
#14472 = AXIS2_PLACEMENT_3D('',#21578,#17409,#17410) ;
#14473 = AXIS2_PLACEMENT_3D('',#21582,#17412,#17413) ;
#14474 = AXIS2_PLACEMENT_3D('',#21583,#17414,#17415) ;
#14475 = AXIS2_PLACEMENT_3D('',#21584,#17416,#17417) ;
#14476 = AXIS2_PLACEMENT_3D('',#21585,#17418,#17419) ;
#14477 = AXIS2_PLACEMENT_3D('',#21588,#17421,#17422) ;
#14478 = AXIS2_PLACEMENT_3D('',#21589,#17423,#17424) ;
#14479 = AXIS2_PLACEMENT_3D('',#21590,#17425,#17426) ;
#14480 = AXIS2_PLACEMENT_3D('',#21592,#17428,#17429) ;
#14481 = AXIS2_PLACEMENT_3D('',#21593,#17430,#17431) ;
#14482 = AXIS2_PLACEMENT_3D('',#21595,#17433,#17434) ;
#14483 = AXIS2_PLACEMENT_3D('',#21596,#17435,#17436) ;
#14484 = AXIS2_PLACEMENT_3D('',#21598,#17438,#17439) ;
#14485 = AXIS2_PLACEMENT_3D('',#21599,#17440,#17441) ;
#14486 = AXIS2_PLACEMENT_3D('',#21602,#17443,#17444) ;
#14487 = AXIS2_PLACEMENT_3D('',#21603,#17445,#17446) ;
#14488 = AXIS2_PLACEMENT_3D('',#21604,#17447,#17448) ;
#14489 = AXIS2_PLACEMENT_3D('',#21608,#17450,#17451) ;
#14490 = AXIS2_PLACEMENT_3D('',#21609,#17452,#17453) ;
#14491 = AXIS2_PLACEMENT_3D('',#21610,#17454,#17455) ;
#14492 = AXIS2_PLACEMENT_3D('',#21611,#17456,#17457) ;
#14493 = AXIS2_PLACEMENT_3D('',#21614,#17459,#17460) ;
#14494 = AXIS2_PLACEMENT_3D('',#21615,#17461,#17462) ;
#14495 = AXIS2_PLACEMENT_3D('',#21616,#17463,#17464) ;
#14496 = AXIS2_PLACEMENT_3D('',#21617,#17465,#17466) ;
#14497 = AXIS2_PLACEMENT_3D('',#21619,#17467,#17468) ;
#14498 = AXIS2_PLACEMENT_3D('',#21621,#17469,#17470) ;
#14499 = AXIS2_PLACEMENT_3D('',#21622,#17471,#17472) ;
#14500 = AXIS2_PLACEMENT_3D('',#21624,#17473,#17474) ;
#14501 = AXIS2_PLACEMENT_3D('',#21625,#17475,#17476) ;
#14502 = AXIS2_PLACEMENT_3D('',#21627,#17477,#17478) ;
#14503 = AXIS2_PLACEMENT_3D('',#21629,#17479,#17480) ;
#14504 = AXIS2_PLACEMENT_3D('',#21630,#17481,#17482) ;
#14505 = AXIS2_PLACEMENT_3D('',#21632,#17483,#17484) ;
#14506 = AXIS2_PLACEMENT_3D('',#21633,#17485,#17486) ;
#14507 = AXIS2_PLACEMENT_3D('',#21636,#17487,#17488) ;
#14508 = AXIS2_PLACEMENT_3D('',#21651,#17489,#17490) ;
#14509 = AXIS2_PLACEMENT_3D('',#21652,#17491,#17492) ;
#14510 = AXIS2_PLACEMENT_3D('',#21653,#17493,#17494) ;
#14511 = AXIS2_PLACEMENT_3D('',#21654,#17495,#17496) ;
#14512 = AXIS2_PLACEMENT_3D('',#21656,#17497,#17498) ;
#14513 = AXIS2_PLACEMENT_3D('',#21658,#17499,#17500) ;
#14514 = AXIS2_PLACEMENT_3D('',#21659,#17501,#17502) ;
#14515 = AXIS2_PLACEMENT_3D('',#21661,#17503,#17504) ;
#14516 = AXIS2_PLACEMENT_3D('',#21689,#17505,#17506) ;
#14517 = AXIS2_PLACEMENT_3D('',#21690,#17507,#17508) ;
#14518 = AXIS2_PLACEMENT_3D('',#21691,#17509,#17510) ;
#14519 = AXIS2_PLACEMENT_3D('',#21692,#17511,#17512) ;
#14520 = AXIS2_PLACEMENT_3D('',#21693,#17513,#17514) ;
#14521 = AXIS2_PLACEMENT_3D('',#21695,#17515,#17516) ;
#14522 = AXIS2_PLACEMENT_3D('',#21697,#17517,#17518) ;
#14523 = AXIS2_PLACEMENT_3D('',#21698,#17519,#17520) ;
#14524 = AXIS2_PLACEMENT_3D('',#21699,#17521,#17522) ;
#14525 = AXIS2_PLACEMENT_3D('',#21701,#17523,#17524) ;
#14526 = AXIS2_PLACEMENT_3D('',#21702,#17525,#17526) ;
#14527 = AXIS2_PLACEMENT_3D('',#21704,#17527,#17528) ;
#14528 = AXIS2_PLACEMENT_3D('',#21705,#17529,#17530) ;
#14529 = AXIS2_PLACEMENT_3D('',#21707,#17531,#17532) ;
#14530 = AXIS2_PLACEMENT_3D('',#21709,#17533,#17534) ;
#14531 = AXIS2_PLACEMENT_3D('',#21710,#17535,#17536) ;
#14532 = AXIS2_PLACEMENT_3D('',#21712,#17537,#17538) ;
#14533 = AXIS2_PLACEMENT_3D('',#21713,#17539,#17540) ;
#14534 = AXIS2_PLACEMENT_3D('',#21715,#17541,#17542) ;
#14535 = AXIS2_PLACEMENT_3D('',#21717,#17543,#17544) ;
#14536 = AXIS2_PLACEMENT_3D('',#21718,#17545,#17546) ;
#14537 = AXIS2_PLACEMENT_3D('',#21720,#17547,#17548) ;
#14538 = AXIS2_PLACEMENT_3D('',#21721,#17549,#17550) ;
#14539 = AXIS2_PLACEMENT_3D('',#21722,#17551,#17552) ;
#14540 = AXIS2_PLACEMENT_3D('',#21724,#17553,#17554) ;
#14541 = AXIS2_PLACEMENT_3D('',#21725,#17555,#17556) ;
#14542 = AXIS2_PLACEMENT_3D('',#21727,#17557,#17558) ;
#14543 = AXIS2_PLACEMENT_3D('',#21729,#17559,#17560) ;
#14544 = AXIS2_PLACEMENT_3D('',#21730,#17561,#17562) ;
#14545 = AXIS2_PLACEMENT_3D('',#21731,#17563,#17564) ;
#14546 = AXIS2_PLACEMENT_3D('',#21733,#17565,#17566) ;
#14547 = AXIS2_PLACEMENT_3D('',#21734,#17567,#17568) ;
#14548 = AXIS2_PLACEMENT_3D('',#21736,#17569,#17570) ;
#14549 = AXIS2_PLACEMENT_3D('',#21737,#17571,#17572) ;
#14550 = AXIS2_PLACEMENT_3D('',#21739,#17573,#17574) ;
#14551 = AXIS2_PLACEMENT_3D('',#21741,#17575,#17576) ;
#14552 = AXIS2_PLACEMENT_3D('',#21742,#17577,#17578) ;
#14553 = AXIS2_PLACEMENT_3D('',#21744,#17579,#17580) ;
#14554 = AXIS2_PLACEMENT_3D('',#21745,#17581,#17582) ;
#14555 = AXIS2_PLACEMENT_3D('',#21747,#17583,#17584) ;
#14556 = AXIS2_PLACEMENT_3D('',#21749,#17585,#17586) ;
#14557 = AXIS2_PLACEMENT_3D('',#21750,#17587,#17588) ;
#14558 = AXIS2_PLACEMENT_3D('',#21752,#17589,#17590) ;
#14559 = AXIS2_PLACEMENT_3D('',#21753,#17591,#17592) ;
#14560 = AXIS2_PLACEMENT_3D('',#21754,#17593,#17594) ;
#14561 = AXIS2_PLACEMENT_3D('',#21756,#17595,#17596) ;
#14562 = AXIS2_PLACEMENT_3D('',#21757,#17597,#17598) ;
#14563 = AXIS2_PLACEMENT_3D('',#21759,#17599,#17600) ;
#14564 = AXIS2_PLACEMENT_3D('',#21761,#17601,#17602) ;
#14565 = AXIS2_PLACEMENT_3D('',#21762,#17603,#17604) ;
#14566 = AXIS2_PLACEMENT_3D('',#21763,#17605,#17606) ;
#14567 = AXIS2_PLACEMENT_3D('',#21765,#17607,#17608) ;
#14568 = AXIS2_PLACEMENT_3D('',#21766,#17609,#17610) ;
#14569 = AXIS2_PLACEMENT_3D('',#21768,#17611,#17612) ;
#14570 = AXIS2_PLACEMENT_3D('',#21769,#17613,#17614) ;
#14571 = AXIS2_PLACEMENT_3D('',#21771,#17615,#17616) ;
#14572 = AXIS2_PLACEMENT_3D('',#21773,#17617,#17618) ;
#14573 = AXIS2_PLACEMENT_3D('',#21774,#17619,#17620) ;
#14574 = AXIS2_PLACEMENT_3D('',#21776,#17621,#17622) ;
#14575 = AXIS2_PLACEMENT_3D('',#21777,#17623,#17624) ;
#14576 = AXIS2_PLACEMENT_3D('',#21779,#17625,#17626) ;
#14577 = AXIS2_PLACEMENT_3D('',#21781,#17627,#17628) ;
#14578 = AXIS2_PLACEMENT_3D('',#21782,#17629,#17630) ;
#14579 = AXIS2_PLACEMENT_3D('',#21784,#17631,#17632) ;
#14580 = AXIS2_PLACEMENT_3D('',#21785,#17633,#17634) ;
#14581 = AXIS2_PLACEMENT_3D('',#21786,#17635,#17636) ;
#14582 = AXIS2_PLACEMENT_3D('',#21788,#17637,#17638) ;
#14583 = AXIS2_PLACEMENT_3D('',#21789,#17639,#17640) ;
#14584 = AXIS2_PLACEMENT_3D('',#21791,#17641,#17642) ;
#14585 = AXIS2_PLACEMENT_3D('',#21793,#17643,#17644) ;
#14586 = AXIS2_PLACEMENT_3D('',#21794,#17645,#17646) ;
#14587 = AXIS2_PLACEMENT_3D('',#21795,#17647,#17648) ;
#14588 = AXIS2_PLACEMENT_3D('',#21797,#17649,#17650) ;
#14589 = AXIS2_PLACEMENT_3D('',#21798,#17651,#17652) ;
#14590 = AXIS2_PLACEMENT_3D('',#21799,#17653,#17654) ;
#14591 = AXIS2_PLACEMENT_3D('',#21801,#17655,#17656) ;
#14592 = AXIS2_PLACEMENT_3D('',#21802,#17657,#17658) ;
#14593 = AXIS2_PLACEMENT_3D('',#21803,#17659,#17660) ;
#14594 = AXIS2_PLACEMENT_3D('',#21805,#17661,#17662) ;
#14595 = AXIS2_PLACEMENT_3D('',#21806,#17663,#17664) ;
#14596 = AXIS2_PLACEMENT_3D('',#21808,#17665,#17666) ;
#14597 = AXIS2_PLACEMENT_3D('',#21809,#17667,#17668) ;
#14598 = AXIS2_PLACEMENT_3D('',#21810,#17669,#17670) ;
#14599 = AXIS2_PLACEMENT_3D('',#21811,#17671,#17672) ;
#14600 = AXIS2_PLACEMENT_3D('',#21813,#17673,#17674) ;
#14601 = AXIS2_PLACEMENT_3D('',#21815,#17675,#17676) ;
#14602 = AXIS2_PLACEMENT_3D('',#21817,#17677,#17678) ;
#14603 = AXIS2_PLACEMENT_3D('',#21818,#17679,#17680) ;
#14604 = AXIS2_PLACEMENT_3D('',#21819,#17681,#17682) ;
#14605 = AXIS2_PLACEMENT_3D('',#21820,#17683,#17684) ;
#14606 = AXIS2_PLACEMENT_3D('',#21822,#17685,#17686) ;
#14607 = AXIS2_PLACEMENT_3D('',#21823,#17687,#17688) ;
#14608 = AXIS2_PLACEMENT_3D('',#21824,#17689,#17690) ;
#14609 = AXIS2_PLACEMENT_3D('',#21826,#17691,#17692) ;
#14610 = AXIS2_PLACEMENT_3D('',#21827,#17693,#17694) ;
#14611 = AXIS2_PLACEMENT_3D('',#21830,#17695,#17696) ;
#14612 = AXIS2_PLACEMENT_3D('',#21832,#17697,#17698) ;
#14613 = AXIS2_PLACEMENT_3D('',#21833,#17699,#17700) ;
#14614 = AXIS2_PLACEMENT_3D('',#21835,#17701,#17702) ;
#14615 = AXIS2_PLACEMENT_3D('',#21836,#17703,#17704) ;
#14616 = AXIS2_PLACEMENT_3D('',#21837,#17705,#17706) ;
#14617 = AXIS2_PLACEMENT_3D('',#21840,#17707,#17708) ;
#14618 = AXIS2_PLACEMENT_3D('',#21842,#17709,#17710) ;
#14619 = AXIS2_PLACEMENT_3D('',#21843,#17711,#17712) ;
#14620 = AXIS2_PLACEMENT_3D('',#21845,#17713,#17714) ;
#14621 = AXIS2_PLACEMENT_3D('',#21847,#17715,#17716) ;
#14622 = AXIS2_PLACEMENT_3D('',#21848,#17717,#17718) ;
#14623 = AXIS2_PLACEMENT_3D('',#21849,#17719,#17720) ;
#14624 = AXIS2_PLACEMENT_3D('',#21850,#17721,#17722) ;
#14625 = AXIS2_PLACEMENT_3D('',#21852,#17723,#17724) ;
#14626 = AXIS2_PLACEMENT_3D('',#21853,#17725,#17726) ;
#14627 = AXIS2_PLACEMENT_3D('',#21854,#17727,#17728) ;
#14628 = AXIS2_PLACEMENT_3D('',#21857,#17729,#17730) ;
#14629 = AXIS2_PLACEMENT_3D('',#21858,#17731,#17732) ;
#14630 = AXIS2_PLACEMENT_3D('',#21859,#17733,#17734) ;
#14631 = AXIS2_PLACEMENT_3D('',#21870,#17735,#17736) ;
#14632 = AXIS2_PLACEMENT_3D('',#21871,#17737,#17738) ;
#14633 = AXIS2_PLACEMENT_3D('',#21873,#17739,#17740) ;
#14634 = AXIS2_PLACEMENT_3D('',#21874,#17741,#17742) ;
#14635 = AXIS2_PLACEMENT_3D('',#21875,#17743,#17744) ;
#14636 = AXIS2_PLACEMENT_3D('',#21878,#17745,#17746) ;
#14637 = AXIS2_PLACEMENT_3D('',#21879,#17747,#17748) ;
#14638 = AXIS2_PLACEMENT_3D('',#21880,#17749,#17750) ;
#14639 = AXIS2_PLACEMENT_3D('',#21882,#17751,#17752) ;
#14640 = AXIS2_PLACEMENT_3D('',#21884,#17753,#17754) ;
#14641 = AXIS2_PLACEMENT_3D('',#21885,#17755,#17756) ;
#14642 = AXIS2_PLACEMENT_3D('',#21888,#17757,#17758) ;
#14643 = AXIS2_PLACEMENT_3D('',#21889,#17759,#17760) ;
#14644 = AXIS2_PLACEMENT_3D('',#21890,#17761,#17762) ;
#14645 = AXIS2_PLACEMENT_3D('',#21893,#17763,#17764) ;
#14646 = AXIS2_PLACEMENT_3D('',#21895,#17765,#17766) ;
#14647 = AXIS2_PLACEMENT_3D('',#21896,#17767,#17768) ;
#14648 = AXIS2_PLACEMENT_3D('',#21898,#17769,#17770) ;
#14649 = AXIS2_PLACEMENT_3D('',#21921,#17771,#17772) ;
#14650 = AXIS2_PLACEMENT_3D('',#21922,#17773,#17774) ;
#14651 = AXIS2_PLACEMENT_3D('',#21923,#17775,#17776) ;
#14652 = AXIS2_PLACEMENT_3D('',#21926,#17777,#17778) ;
#14653 = AXIS2_PLACEMENT_3D('',#21928,#17779,#17780) ;
#14654 = AXIS2_PLACEMENT_3D('',#21930,#17781,#17782) ;
#14655 = AXIS2_PLACEMENT_3D('',#21931,#17783,#17784) ;
#14656 = AXIS2_PLACEMENT_3D('',#21932,#17785,#17786) ;
#14657 = AXIS2_PLACEMENT_3D('',#21935,#17787,#17788) ;
#14658 = AXIS2_PLACEMENT_3D('',#21937,#17789,#17790) ;
#14659 = AXIS2_PLACEMENT_3D('',#21939,#17791,#17792) ;
#14660 = AXIS2_PLACEMENT_3D('',#21940,#17793,#17794) ;
#14661 = AXIS2_PLACEMENT_3D('',#21941,#17795,#17796) ;
#14662 = AXIS2_PLACEMENT_3D('',#21944,#17797,#17798) ;
#14663 = AXIS2_PLACEMENT_3D('',#21946,#17799,#17800) ;
#14664 = AXIS2_PLACEMENT_3D('',#21948,#17801,#17802) ;
#14665 = AXIS2_PLACEMENT_3D('',#21949,#17803,#17804) ;
#14666 = AXIS2_PLACEMENT_3D('',#21950,#17805,#17806) ;
#14667 = AXIS2_PLACEMENT_3D('',#21953,#17807,#17808) ;
#14668 = AXIS2_PLACEMENT_3D('',#21955,#17809,#17810) ;
#14669 = AXIS2_PLACEMENT_3D('',#21957,#17811,#17812) ;
#14670 = AXIS2_PLACEMENT_3D('',#21958,#17813,#17814) ;
#14671 = AXIS2_PLACEMENT_3D('',#21959,#17815,#17816) ;
#14672 = AXIS2_PLACEMENT_3D('',#21962,#17817,#17818) ;
#14673 = AXIS2_PLACEMENT_3D('',#21964,#17819,#17820) ;
#14674 = AXIS2_PLACEMENT_3D('',#21966,#17821,#17822) ;
#14675 = AXIS2_PLACEMENT_3D('',#21967,#17823,#17824) ;
#14676 = AXIS2_PLACEMENT_3D('',#21968,#17825,#17826) ;
#14677 = AXIS2_PLACEMENT_3D('',#21971,#17827,#17828) ;
#14678 = AXIS2_PLACEMENT_3D('',#21973,#17829,#17830) ;
#14679 = AXIS2_PLACEMENT_3D('',#21975,#17831,#17832) ;
#14680 = AXIS2_PLACEMENT_3D('',#21976,#17833,#17834) ;
#14681 = AXIS2_PLACEMENT_3D('',#21977,#17835,#17836) ;
#14682 = AXIS2_PLACEMENT_3D('',#21980,#17837,#17838) ;
#14683 = AXIS2_PLACEMENT_3D('',#21981,#17839,#17840) ;
#14684 = AXIS2_PLACEMENT_3D('',#21982,#17841,#17842) ;
#14685 = AXIS2_PLACEMENT_3D('',#21985,#17843,#17844) ;
#14686 = AXIS2_PLACEMENT_3D('',#21987,#17845,#17846) ;
#14687 = AXIS2_PLACEMENT_3D('',#21989,#17847,#17848) ;
#14688 = AXIS2_PLACEMENT_3D('',#21990,#17849,#17850) ;
#14689 = AXIS2_PLACEMENT_3D('',#21991,#17851,#17852) ;
#14690 = AXIS2_PLACEMENT_3D('',#21993,#17853,#17854) ;
#14691 = AXIS2_PLACEMENT_3D('',#22026,#17856,#17857) ;
#14692 = AXIS2_PLACEMENT_3D('',#22028,#17858,#17859) ;
#14693 = AXIS2_PLACEMENT_3D('',#22032,#17861,#17862) ;
#14694 = AXIS2_PLACEMENT_3D('',#22034,#17863,#17864) ;
#14695 = AXIS2_PLACEMENT_3D('',#22036,#17865,#17866) ;
#14696 = AXIS2_PLACEMENT_3D('',#22037,#17867,#17868) ;
#14697 = AXIS2_PLACEMENT_3D('',#22038,#17869,#17870) ;
#14698 = AXIS2_PLACEMENT_3D('',#22040,#17871,#17872) ;
#14699 = AXIS2_PLACEMENT_3D('',#22041,#17873,#17874) ;
#14700 = AXIS2_PLACEMENT_3D('',#22045,#17876,#17877) ;
#14701 = AXIS2_PLACEMENT_3D('',#22047,#17878,#17879) ;
#14702 = AXIS2_PLACEMENT_3D('',#22048,#17880,#17881) ;
#14703 = AXIS2_PLACEMENT_3D('',#22049,#17882,#17883) ;
#14704 = AXIS2_PLACEMENT_3D('',#22050,#17884,#17885) ;
#14705 = AXIS2_PLACEMENT_3D('',#22084,#17886,#17887) ;
#14706 = AXIS2_PLACEMENT_3D('',#22085,#17888,#17889) ;
#14707 = AXIS2_PLACEMENT_3D('',#22087,#17890,#17891) ;
#14708 = AXIS2_PLACEMENT_3D('',#22089,#17893,#17894) ;
#14709 = AXIS2_PLACEMENT_3D('',#22090,#17895,#17896) ;
#14710 = AXIS2_PLACEMENT_3D('',#22091,#17897,#17898) ;
#14711 = AXIS2_PLACEMENT_3D('',#22093,#17900,#17901) ;
#14712 = AXIS2_PLACEMENT_3D('',#22094,#17902,#17903) ;
#14713 = AXIS2_PLACEMENT_3D('',#22098,#17905,#17906) ;
#14714 = AXIS2_PLACEMENT_3D('',#22100,#17907,#17908) ;
#14715 = AXIS2_PLACEMENT_3D('',#22101,#17909,#17910) ;
#14716 = AXIS2_PLACEMENT_3D('',#22102,#17911,#17912) ;
#14717 = AXIS2_PLACEMENT_3D('',#22104,#17913,#17914) ;
#14718 = AXIS2_PLACEMENT_3D('',#22108,#17916,#17917) ;
#14719 = AXIS2_PLACEMENT_3D('',#22110,#17918,#17919) ;
#14720 = AXIS2_PLACEMENT_3D('',#22111,#17920,#17921) ;
#14721 = AXIS2_PLACEMENT_3D('',#22112,#17922,#17923) ;
#14722 = AXIS2_PLACEMENT_3D('',#22113,#17924,#17925) ;
#14723 = AXIS2_PLACEMENT_3D('',#22115,#17926,#17927) ;
#14724 = AXIS2_PLACEMENT_3D('',#22117,#17929,#17930) ;
#14725 = AXIS2_PLACEMENT_3D('',#22118,#17931,#17932) ;
#14726 = AXIS2_PLACEMENT_3D('',#22119,#17933,#17934) ;
#14727 = AXIS2_PLACEMENT_3D('',#22121,#17936,#17937) ;
#14728 = AXIS2_PLACEMENT_3D('',#22122,#17938,#17939) ;
#14729 = AXIS2_PLACEMENT_3D('',#22126,#17941,#17942) ;
#14730 = AXIS2_PLACEMENT_3D('',#22128,#17943,#17944) ;
#14731 = AXIS2_PLACEMENT_3D('',#22129,#17945,#17946) ;
#14732 = AXIS2_PLACEMENT_3D('',#22130,#17947,#17948) ;
#14733 = AXIS2_PLACEMENT_3D('',#22132,#17949,#17950) ;
#14734 = AXIS2_PLACEMENT_3D('',#22136,#17952,#17953) ;
#14735 = AXIS2_PLACEMENT_3D('',#22138,#17954,#17955) ;
#14736 = AXIS2_PLACEMENT_3D('',#22139,#17956,#17957) ;
#14737 = AXIS2_PLACEMENT_3D('',#22140,#17958,#17959) ;
#14738 = AXIS2_PLACEMENT_3D('',#22141,#17960,#17961) ;
#14739 = AXIS2_PLACEMENT_3D('',#22143,#17962,#17963) ;
#14740 = AXIS2_PLACEMENT_3D('',#22145,#17965,#17966) ;
#14741 = AXIS2_PLACEMENT_3D('',#22146,#17967,#17968) ;
#14742 = AXIS2_PLACEMENT_3D('',#22147,#17969,#17970) ;
#14743 = AXIS2_PLACEMENT_3D('',#22149,#17972,#17973) ;
#14744 = AXIS2_PLACEMENT_3D('',#22150,#17974,#17975) ;
#14745 = AXIS2_PLACEMENT_3D('',#22154,#17977,#17978) ;
#14746 = AXIS2_PLACEMENT_3D('',#22156,#17979,#17980) ;
#14747 = AXIS2_PLACEMENT_3D('',#22157,#17981,#17982) ;
#14748 = AXIS2_PLACEMENT_3D('',#22158,#17983,#17984) ;
#14749 = AXIS2_PLACEMENT_3D('',#22160,#17985,#17986) ;
#14750 = AXIS2_PLACEMENT_3D('',#22164,#17988,#17989) ;
#14751 = AXIS2_PLACEMENT_3D('',#22166,#17990,#17991) ;
#14752 = AXIS2_PLACEMENT_3D('',#22167,#17992,#17993) ;
#14753 = AXIS2_PLACEMENT_3D('',#22168,#17994,#17995) ;
#14754 = AXIS2_PLACEMENT_3D('',#22169,#17996,#17997) ;
#14755 = AXIS2_PLACEMENT_3D('',#22171,#17998,#17999) ;
#14756 = AXIS2_PLACEMENT_3D('',#22174,#18001,#18002) ;
#14757 = AXIS2_PLACEMENT_3D('',#22175,#18003,#18004) ;
#14758 = AXIS2_PLACEMENT_3D('',#22176,#18005,#18006) ;
#14759 = AXIS2_PLACEMENT_3D('',#22177,#18007,#18008) ;
#14760 = AXIS2_PLACEMENT_3D('',#22178,#18009,#18010) ;
#14761 = AXIS2_PLACEMENT_3D('',#22181,#18012,#18013) ;
#14762 = AXIS2_PLACEMENT_3D('',#22182,#18014,#18015) ;
#14763 = AXIS2_PLACEMENT_3D('',#22183,#18016,#18017) ;
#14764 = AXIS2_PLACEMENT_3D('',#22184,#18018,#18019) ;
#14765 = AXIS2_PLACEMENT_3D('',#22185,#18020,#18021) ;
#14766 = AXIS2_PLACEMENT_3D('',#22186,#18022,#18023) ;
#14767 = AXIS2_PLACEMENT_3D('',#22187,#18024,#18025) ;
#14768 = AXIS2_PLACEMENT_3D('',#22188,#18026,#18027) ;
#14769 = AXIS2_PLACEMENT_3D('',#22189,#18028,#18029) ;
#14770 = AXIS2_PLACEMENT_3D('',#22191,#18030,#18031) ;
#14771 = AXIS2_PLACEMENT_3D('',#22192,#18032,#18033) ;
#14772 = AXIS2_PLACEMENT_3D('',#22193,#18034,#18035) ;
#14773 = AXIS2_PLACEMENT_3D('',#22195,#18037,#18038) ;
#14774 = AXIS2_PLACEMENT_3D('',#22197,#18039,#18040) ;
#14775 = AXIS2_PLACEMENT_3D('',#22198,#18041,#18042) ;
#14776 = AXIS2_PLACEMENT_3D('',#22199,#18043,#18044) ;
#14777 = AXIS2_PLACEMENT_3D('',#22201,#18045,#18046) ;
#14778 = AXIS2_PLACEMENT_3D('',#22202,#18047,#18048) ;
#14779 = AXIS2_PLACEMENT_3D('',#22203,#18049,#18050) ;
#14780 = AXIS2_PLACEMENT_3D('',#22205,#18051,#18052) ;
#14781 = AXIS2_PLACEMENT_3D('',#22206,#18053,#18054) ;
#14782 = AXIS2_PLACEMENT_3D('',#22207,#18055,#18056) ;
#14783 = AXIS2_PLACEMENT_3D('',#22209,#18057,#18058) ;
#14784 = AXIS2_PLACEMENT_3D('',#22211,#18059,#18060) ;
#14785 = AXIS2_PLACEMENT_3D('',#22212,#18061,#18062) ;
#14786 = AXIS2_PLACEMENT_3D('',#22214,#18063,#18064) ;
#14787 = AXIS2_PLACEMENT_3D('',#22215,#18065,#18066) ;
#14788 = AXIS2_PLACEMENT_3D('',#22217,#18067,#18068) ;
#14789 = AXIS2_PLACEMENT_3D('',#22219,#18069,#18070) ;
#14790 = AXIS2_PLACEMENT_3D('',#22220,#18071,#18072) ;
#14791 = AXIS2_PLACEMENT_3D('',#22222,#18073,#18074) ;
#14792 = AXIS2_PLACEMENT_3D('',#22223,#18075,#18076) ;
#14793 = AXIS2_PLACEMENT_3D('',#22225,#18077,#18078) ;
#14794 = AXIS2_PLACEMENT_3D('',#22227,#18079,#18080) ;
#14795 = AXIS2_PLACEMENT_3D('',#22228,#18081,#18082) ;
#14796 = AXIS2_PLACEMENT_3D('',#22230,#18083,#18084) ;
#14797 = AXIS2_PLACEMENT_3D('',#22231,#18085,#18086) ;
#14798 = AXIS2_PLACEMENT_3D('',#22233,#18087,#18088) ;
#14799 = AXIS2_PLACEMENT_3D('',#22235,#18089,#18090) ;
#14800 = AXIS2_PLACEMENT_3D('',#22236,#18091,#18092) ;
#14801 = AXIS2_PLACEMENT_3D('',#22238,#18093,#18094) ;
#14802 = AXIS2_PLACEMENT_3D('',#22239,#18095,#18096) ;
#14803 = AXIS2_PLACEMENT_3D('',#22240,#18097,#18098) ;
#14804 = AXIS2_PLACEMENT_3D('',#22243,#18099,#18100) ;
#14805 = AXIS2_PLACEMENT_3D('',#22247,#18102,#18103) ;
#14806 = AXIS2_PLACEMENT_3D('',#22249,#18105,#18106) ;
#14807 = AXIS2_PLACEMENT_3D('',#22255,#18110,#18111) ;
#14808 = AXIS2_PLACEMENT_3D('',#22257,#18112,#18113) ;
#14809 = AXIS2_PLACEMENT_3D('',#22259,#18114,#18115) ;
#14810 = AXIS2_PLACEMENT_3D('',#22261,#18117,#18118) ;
#14811 = AXIS2_PLACEMENT_3D('',#22264,#18121,#18122) ;
#14812 = AXIS2_PLACEMENT_3D('',#22266,#18123,#18124) ;
#14813 = AXIS2_PLACEMENT_3D('',#22269,#18126,#18127) ;
#14814 = AXIS2_PLACEMENT_3D('',#22270,#18128,#18129) ;
#14815 = AXIS2_PLACEMENT_3D('',#22273,#18130,#18131) ;
#14816 = AXIS2_PLACEMENT_3D('',#22277,#18133,#18134) ;
#14817 = AXIS2_PLACEMENT_3D('',#22279,#18136,#18137) ;
#14818 = AXIS2_PLACEMENT_3D('',#22285,#18141,#18142) ;
#14819 = AXIS2_PLACEMENT_3D('',#22287,#18143,#18144) ;
#14820 = AXIS2_PLACEMENT_3D('',#22289,#18145,#18146) ;
#14821 = AXIS2_PLACEMENT_3D('',#22291,#18148,#18149) ;
#14822 = AXIS2_PLACEMENT_3D('',#22294,#18152,#18153) ;
#14823 = AXIS2_PLACEMENT_3D('',#22296,#18154,#18155) ;
#14824 = AXIS2_PLACEMENT_3D('',#22299,#18157,#18158) ;
#14825 = AXIS2_PLACEMENT_3D('',#22300,#18159,#18160) ;
#14826 = AXIS2_PLACEMENT_3D('',#22309,#18165,#18166) ;
#14827 = AXIS2_PLACEMENT_3D('',#22315,#18170,#18171) ;
#14828 = AXIS2_PLACEMENT_3D('',#22321,#18175,#18176) ;
#14829 = AXIS2_PLACEMENT_3D('',#22327,#18180,#18181) ;
#14830 = AXIS2_PLACEMENT_3D('',#22331,#18184,#18185) ;
#14831 = AXIS2_PLACEMENT_3D('',#22335,#18188,#18189) ;
#14832 = AXIS2_PLACEMENT_3D('',#22337,#18191,#18192) ;
#14833 = AXIS2_PLACEMENT_3D('',#22338,#18193,#18194) ;
#14834 = AXIS2_PLACEMENT_3D('',#22339,#18195,#18196) ;
#14835 = AXIS2_PLACEMENT_3D('',#22340,#18197,#18198) ;
#14836 = AXIS2_PLACEMENT_3D('',#22341,#18199,#18200) ;
#14837 = AXIS2_PLACEMENT_3D('',#22342,#18201,#18202) ;
#14838 = AXIS2_PLACEMENT_3D('',#22343,#18203,#18204) ;
#14839 = AXIS2_PLACEMENT_3D('',#22344,#18205,#18206) ;
#14840 = AXIS2_PLACEMENT_3D('',#22345,#18207,#18208) ;
#14841 = AXIS2_PLACEMENT_3D('',#22346,#18209,#18210) ;
#14842 = AXIS2_PLACEMENT_3D('',#22347,#18211,#18212) ;
#14843 = AXIS2_PLACEMENT_3D('',#22348,#18213,#18214) ;
#14844 = AXIS2_PLACEMENT_3D('',#22349,#18215,#18216) ;
#14845 = AXIS2_PLACEMENT_3D('',#22350,#18217,#18218) ;
#14846 = AXIS2_PLACEMENT_3D('',#22351,#18219,#18220) ;
#14847 = AXIS2_PLACEMENT_3D('',#22352,#18221,#18222) ;
#14848 = AXIS2_PLACEMENT_3D('',#22353,#18223,#18224) ;
#14849 = AXIS2_PLACEMENT_3D('',#22354,#18225,#18226) ;
#14850 = AXIS2_PLACEMENT_3D('',#22355,#18227,#18228) ;
#14851 = AXIS2_PLACEMENT_3D('',#22356,#18229,#18230) ;
#14852 = AXIS2_PLACEMENT_3D('',#22357,#18231,#18232) ;
#14853 = AXIS2_PLACEMENT_3D('',#22358,#18233,#18234) ;
#14854 = AXIS2_PLACEMENT_3D('',#22359,#18235,#18236) ;
#14855 = AXIS2_PLACEMENT_3D('',#22360,#18237,#18238) ;
#14856 = AXIS2_PLACEMENT_3D('',#22361,#18239,#18240) ;
#14857 = AXIS2_PLACEMENT_3D('',#22713,#18241,#18242) ;
#14858 = AXIS2_PLACEMENT_3D('',#22716,#18243,#18244) ;
#14859 = AXIS2_PLACEMENT_3D('',#22718,#18245,#18246) ;
#14860 = AXIS2_PLACEMENT_3D('',#22720,#18247,#18248) ;
#14861 = AXIS2_PLACEMENT_3D('',#22721,#18249,#18250) ;
#14862 = AXIS2_PLACEMENT_3D('',#22722,#18251,#18252) ;
#14863 = AXIS2_PLACEMENT_3D('',#22839,#18261,#18262) ;
#14864 = AXIS2_PLACEMENT_3D('',#22840,#18263,#18264) ;
#14865 = AXIS2_PLACEMENT_3D('',#22842,#18265,#18266) ;
#14866 = AXIS2_PLACEMENT_3D('',#22845,#18268,#18269) ;
#14867 = AXIS2_PLACEMENT_3D('',#22846,#18270,#18271) ;
#14868 = AXIS2_PLACEMENT_3D('',#22847,#18272,#18273) ;
#14869 = AXIS2_PLACEMENT_3D('',#22856,#18278,#18279) ;
#14870 = AXIS2_PLACEMENT_3D('',#22862,#18283,#18284) ;
#14871 = AXIS2_PLACEMENT_3D('',#22866,#18287,#18288) ;
#14872 = AXIS2_PLACEMENT_3D('',#22870,#18291,#18292) ;
#14873 = AXIS2_PLACEMENT_3D('',#22872,#18294,#18295) ;
#14874 = AXIS2_PLACEMENT_3D('',#22881,#18300,#18301) ;
#14875 = AXIS2_PLACEMENT_3D('',#22887,#18305,#18306) ;
#14876 = AXIS2_PLACEMENT_3D('',#22891,#18309,#18310) ;
#14877 = AXIS2_PLACEMENT_3D('',#22895,#18313,#18314) ;
#14878 = AXIS2_PLACEMENT_3D('',#22897,#18316,#18317) ;
#14879 = AXIS2_PLACEMENT_3D('',#22906,#18322,#18323) ;
#14880 = AXIS2_PLACEMENT_3D('',#22915,#18328,#18329) ;
#14881 = AXIS2_PLACEMENT_3D('',#22918,#18332,#18333) ;
#14882 = AXIS2_PLACEMENT_3D('',#22920,#18335,#18336) ;
#14883 = AXIS2_PLACEMENT_3D('',#22922,#18338,#18339) ;
#14884 = AXIS2_PLACEMENT_3D('',#22923,#18340,#18341) ;
#14885 = AXIS2_PLACEMENT_3D('',#22924,#18342,#18343) ;
#14886 = AXIS2_PLACEMENT_3D('',#22941,#18352,#18353) ;
#14887 = AXIS2_PLACEMENT_3D('',#22950,#18358,#18359) ;
#14888 = AXIS2_PLACEMENT_3D('',#22952,#18360,#18361) ;
#14889 = AXIS2_PLACEMENT_3D('',#22960,#18366,#18367) ;
#14890 = AXIS2_PLACEMENT_3D('',#22962,#18368,#18369) ;
#14891 = AXIS2_PLACEMENT_3D('',#22970,#18374,#18375) ;
#14892 = AXIS2_PLACEMENT_3D('',#22978,#18379,#18380) ;
#14893 = AXIS2_PLACEMENT_3D('',#22980,#18382,#18383) ;
#14894 = AXIS2_PLACEMENT_3D('',#22982,#18384,#18385) ;
#14895 = AXIS2_PLACEMENT_3D('',#22984,#18387,#18388) ;
#14896 = AXIS2_PLACEMENT_3D('',#22985,#18389,#18390) ;
#14897 = AXIS2_PLACEMENT_3D('',#22986,#18391,#18392) ;
#14898 = AXIS2_PLACEMENT_3D('',#22988,#18393,#18394) ;
#14899 = AXIS2_PLACEMENT_3D('',#22990,#18396,#18397) ;
#14900 = AXIS2_PLACEMENT_3D('',#22992,#18398,#18399) ;
#14901 = AXIS2_PLACEMENT_3D('',#22994,#18401,#18402) ;
#14902 = AXIS2_PLACEMENT_3D('',#22998,#18405,#18406) ;
#14903 = AXIS2_PLACEMENT_3D('',#23003,#18409,#18410) ;
#14904 = AXIS2_PLACEMENT_3D('',#23004,#18411,#18412) ;
#14905 = AXIS2_PLACEMENT_3D('',#23010,#18416,#18417) ;
#14906 = AXIS2_PLACEMENT_3D('',#23013,#18419,#18420) ;
#14907 = AXIS2_PLACEMENT_3D('',#23014,#18421,#18422) ;
#14908 = AXIS2_PLACEMENT_3D('',#23016,#18423,#18424) ;
#14909 = AXIS2_PLACEMENT_3D('',#23018,#18426,#18427) ;
#14910 = AXIS2_PLACEMENT_3D('',#23020,#18428,#18429) ;
#14911 = AXIS2_PLACEMENT_3D('',#23021,#18430,#18431) ;
#14912 = AXIS2_PLACEMENT_3D('',#23022,#18432,#18433) ;
#14913 = AXIS2_PLACEMENT_3D('',#23024,#18434,#18435) ;
#14914 = AXIS2_PLACEMENT_3D('',#23026,#18437,#18438) ;
#14915 = AXIS2_PLACEMENT_3D('',#23027,#18439,#18440) ;
#14916 = AXIS2_PLACEMENT_3D('',#23028,#18441,#18442) ;
#14917 = AXIS2_PLACEMENT_3D('',#23030,#18443,#18444) ;
#14918 = AXIS2_PLACEMENT_3D('',#23086,#18446,#18447) ;
#14919 = AXIS2_PLACEMENT_3D('',#23088,#18448,#18449) ;
#14920 = AXIS2_PLACEMENT_3D('',#23091,#18451,#18452) ;
#14921 = AXIS2_PLACEMENT_3D('',#23092,#18453,#18454) ;
#14922 = AXIS2_PLACEMENT_3D('',#23094,#18455,#18456) ;
#14923 = AXIS2_PLACEMENT_3D('',#23097,#18458,#18459) ;
#14924 = AXIS2_PLACEMENT_3D('',#23098,#18460,#18461) ;
#14925 = AXIS2_PLACEMENT_3D('',#23100,#18462,#18463) ;
#14926 = AXIS2_PLACEMENT_3D('',#23103,#18465,#18466) ;
#14927 = AXIS2_PLACEMENT_3D('',#23142,#18468,#18469) ;
#14928 = AXIS2_PLACEMENT_3D('',#23143,#18470,#18471) ;
#14929 = AXIS2_PLACEMENT_3D('',#23144,#18472,#18473) ;
#14930 = AXIS2_PLACEMENT_3D('',#23145,#18474,#18475) ;
#14931 = AXIS2_PLACEMENT_3D('',#23146,#18476,#18477) ;
#14932 = AXIS2_PLACEMENT_3D('',#23149,#18479,#18480) ;
#14933 = AXIS2_PLACEMENT_3D('',#23150,#18481,#18482) ;
#14934 = AXIS2_PLACEMENT_3D('',#23159,#18487,#18488) ;
#14935 = AXIS2_PLACEMENT_3D('',#23168,#18493,#18494) ;
#14936 = AXIS2_PLACEMENT_3D('',#23171,#18497,#18498) ;
#14937 = AXIS2_PLACEMENT_3D('',#23173,#18500,#18501) ;
#14938 = AXIS2_PLACEMENT_3D('',#23175,#18503,#18504) ;
#14939 = AXIS2_PLACEMENT_3D('',#23176,#18505,#18506) ;
#14940 = AXIS2_PLACEMENT_3D('',#23177,#18507,#18508) ;
#14941 = AXIS2_PLACEMENT_3D('',#23179,#18509,#18510) ;
#14942 = AXIS2_PLACEMENT_3D('',#23182,#18512,#18513) ;
#14943 = AXIS2_PLACEMENT_3D('',#23183,#18514,#18515) ;
#14944 = AXIS2_PLACEMENT_3D('',#23186,#18516,#18517) ;
#14945 = AXIS2_PLACEMENT_3D('',#23190,#18519,#18520) ;
#14946 = AXIS2_PLACEMENT_3D('',#23192,#18522,#18523) ;
#14947 = AXIS2_PLACEMENT_3D('',#23194,#18524,#18525) ;
#14948 = AXIS2_PLACEMENT_3D('',#23196,#18526,#18527) ;
#14949 = AXIS2_PLACEMENT_3D('',#23198,#18528,#18529) ;
#14950 = AXIS2_PLACEMENT_3D('',#23200,#18530,#18531) ;
#14951 = AXIS2_PLACEMENT_3D('',#23202,#18532,#18533) ;
#14952 = AXIS2_PLACEMENT_3D('',#23204,#18534,#18535) ;
#14953 = AXIS2_PLACEMENT_3D('',#23206,#18536,#18537) ;
#14954 = AXIS2_PLACEMENT_3D('',#23208,#18538,#18539) ;
#14955 = AXIS2_PLACEMENT_3D('',#23210,#18540,#18541) ;
#14956 = AXIS2_PLACEMENT_3D('',#23212,#18542,#18543) ;
#14957 = AXIS2_PLACEMENT_3D('',#23214,#18544,#18545) ;
#14958 = AXIS2_PLACEMENT_3D('',#23216,#18546,#18547) ;
#14959 = AXIS2_PLACEMENT_3D('',#23218,#18548,#18549) ;
#14960 = AXIS2_PLACEMENT_3D('',#23220,#18550,#18551) ;
#14961 = AXIS2_PLACEMENT_3D('',#23221,#18552,#18553) ;
#14962 = AXIS2_PLACEMENT_3D('',#23222,#18554,#18555) ;
#14963 = AXIS2_PLACEMENT_3D('',#23224,#18556,#18557) ;
#14964 = AXIS2_PLACEMENT_3D('',#23226,#18559,#18560) ;
#14965 = AXIS2_PLACEMENT_3D('',#23228,#18561,#18562) ;
#14966 = AXIS2_PLACEMENT_3D('',#23230,#18564,#18565) ;
#14967 = AXIS2_PLACEMENT_3D('',#23232,#18566,#18567) ;
#14968 = AXIS2_PLACEMENT_3D('',#23234,#18569,#18570) ;
#14969 = AXIS2_PLACEMENT_3D('',#23236,#18571,#18572) ;
#14970 = AXIS2_PLACEMENT_3D('',#23238,#18574,#18575) ;
#14971 = AXIS2_PLACEMENT_3D('',#23240,#18576,#18577) ;
#14972 = AXIS2_PLACEMENT_3D('',#23242,#18579,#18580) ;
#14973 = AXIS2_PLACEMENT_3D('',#23244,#18581,#18582) ;
#14974 = AXIS2_PLACEMENT_3D('',#23246,#18584,#18585) ;
#14975 = AXIS2_PLACEMENT_3D('',#23248,#18586,#18587) ;
#14976 = AXIS2_PLACEMENT_3D('',#23250,#18589,#18590) ;
#14977 = AXIS2_PLACEMENT_3D('',#23252,#18591,#18592) ;
#14978 = AXIS2_PLACEMENT_3D('',#23254,#18594,#18595) ;
#14979 = AXIS2_PLACEMENT_3D('',#23256,#18596,#18597) ;
#14980 = AXIS2_PLACEMENT_3D('',#23258,#18599,#18600) ;
#14981 = AXIS2_PLACEMENT_3D('',#23260,#18601,#18602) ;
#14982 = AXIS2_PLACEMENT_3D('',#23262,#18604,#18605) ;
#14983 = AXIS2_PLACEMENT_3D('',#23264,#18606,#18607) ;
#14984 = AXIS2_PLACEMENT_3D('',#23266,#18609,#18610) ;
#14985 = AXIS2_PLACEMENT_3D('',#23268,#18611,#18612) ;
#14986 = AXIS2_PLACEMENT_3D('',#23270,#18614,#18615) ;
#14987 = AXIS2_PLACEMENT_3D('',#23272,#18616,#18617) ;
#14988 = AXIS2_PLACEMENT_3D('',#23274,#18619,#18620) ;
#14989 = AXIS2_PLACEMENT_3D('',#23276,#18621,#18622) ;
#14990 = AXIS2_PLACEMENT_3D('',#23278,#18624,#18625) ;
#14991 = AXIS2_PLACEMENT_3D('',#23279,#18626,#18627) ;
#14992 = AXIS2_PLACEMENT_3D('',#23280,#18628,#18629) ;
#14993 = AXIS2_PLACEMENT_3D('',#23281,#18630,#18631) ;
#14994 = AXIS2_PLACEMENT_3D('',#23282,#18632,#18633) ;
#14995 = AXIS2_PLACEMENT_3D('',#23284,#18634,#18635) ;
#14996 = AXIS2_PLACEMENT_3D('',#23287,#18637,#18638) ;
#14997 = AXIS2_PLACEMENT_3D('',#23288,#18639,#18640) ;
#14998 = AXIS2_PLACEMENT_3D('',#23289,#18641,#18642) ;
#14999 = AXIS2_PLACEMENT_3D('',#23290,#18643,#18644) ;
#15000 = AXIS2_PLACEMENT_3D('',#23291,#18645,#18646) ;
#15001 = AXIS2_PLACEMENT_3D('',#23293,#18647,#18648) ;
#15002 = AXIS2_PLACEMENT_3D('',#23296,#18650,#18651) ;
#15003 = AXIS2_PLACEMENT_3D('',#23297,#18652,#18653) ;
#15004 = AXIS2_PLACEMENT_3D('',#23299,#18654,#18655) ;
#15005 = AXIS2_PLACEMENT_3D('',#23302,#18657,#18658) ;
#15006 = AXIS2_PLACEMENT_3D('',#23303,#18659,#18660) ;
#15007 = AXIS2_PLACEMENT_3D('',#23304,#18661,#18662) ;
#15008 = AXIS2_PLACEMENT_3D('',#23305,#18663,#18664) ;
#15009 = AXIS2_PLACEMENT_3D('',#23306,#18665,#18666) ;
#15010 = AXIS2_PLACEMENT_3D('',#23308,#18667,#18668) ;
#15011 = AXIS2_PLACEMENT_3D('',#23311,#18670,#18671) ;
#15012 = AXIS2_PLACEMENT_3D('',#23312,#18672,#18673) ;
#15013 = AXIS2_PLACEMENT_3D('',#23314,#18674,#18675) ;
#15014 = AXIS2_PLACEMENT_3D('',#23317,#18677,#18678) ;
#15015 = AXIS2_PLACEMENT_3D('',#23318,#18679,#18680) ;
#15016 = AXIS2_PLACEMENT_3D('',#23319,#18681,#18682) ;
#15017 = AXIS2_PLACEMENT_3D('',#23322,#18683,#18684) ;
#15018 = AXIS2_PLACEMENT_3D('',#23328,#18688,#18689) ;
#15019 = AXIS2_PLACEMENT_3D('',#23334,#18693,#18694) ;
#15020 = AXIS2_PLACEMENT_3D('',#23340,#18698,#18699) ;
#15021 = AXIS2_PLACEMENT_3D('',#23341,#18700,#18701) ;
#15022 = AXIS2_PLACEMENT_3D('',#23343,#18703,#18704) ;
#15023 = AXIS2_PLACEMENT_3D('',#23344,#18705,#18706) ;
#15024 = AXIS2_PLACEMENT_3D('',#23347,#18707,#18708) ;
#15025 = AXIS2_PLACEMENT_3D('',#23353,#18712,#18713) ;
#15026 = AXIS2_PLACEMENT_3D('',#23359,#18717,#18718) ;
#15027 = AXIS2_PLACEMENT_3D('',#23365,#18722,#18723) ;
#15028 = AXIS2_PLACEMENT_3D('',#23366,#18724,#18725) ;
#15029 = AXIS2_PLACEMENT_3D('',#23368,#18727,#18728) ;
#15030 = AXIS2_PLACEMENT_3D('',#23369,#18729,#18730) ;
#15031 = AXIS2_PLACEMENT_3D('',#23372,#18731,#18732) ;
#15032 = AXIS2_PLACEMENT_3D('',#23378,#18736,#18737) ;
#15033 = AXIS2_PLACEMENT_3D('',#23384,#18741,#18742) ;
#15034 = AXIS2_PLACEMENT_3D('',#23390,#18746,#18747) ;
#15035 = AXIS2_PLACEMENT_3D('',#23391,#18748,#18749) ;
#15036 = AXIS2_PLACEMENT_3D('',#23393,#18751,#18752) ;
#15037 = AXIS2_PLACEMENT_3D('',#23394,#18753,#18754) ;
#15038 = AXIS2_PLACEMENT_3D('',#23397,#18755,#18756) ;
#15039 = AXIS2_PLACEMENT_3D('',#23403,#18760,#18761) ;
#15040 = AXIS2_PLACEMENT_3D('',#23409,#18765,#18766) ;
#15041 = AXIS2_PLACEMENT_3D('',#23415,#18770,#18771) ;
#15042 = AXIS2_PLACEMENT_3D('',#23416,#18772,#18773) ;
#15043 = AXIS2_PLACEMENT_3D('',#23418,#18775,#18776) ;
#15044 = AXIS2_PLACEMENT_3D('',#23419,#18777,#18778) ;
#15045 = AXIS2_PLACEMENT_3D('',#23422,#18779,#18780) ;
#15046 = AXIS2_PLACEMENT_3D('',#23429,#18784,#18785) ;
#15047 = AXIS2_PLACEMENT_3D('',#23430,#18786,#18787) ;
#15048 = AXIS2_PLACEMENT_3D('',#23436,#18791,#18792) ;
#15049 = AXIS2_PLACEMENT_3D('',#23442,#18796,#18797) ;
#15050 = AXIS2_PLACEMENT_3D('',#23444,#18798,#18799) ;
#15051 = AXIS2_PLACEMENT_3D('',#23446,#18801,#18802) ;
#15052 = AXIS2_PLACEMENT_3D('',#23447,#18803,#18804) ;
#15053 = AXIS2_PLACEMENT_3D('',#23448,#18805,#18806) ;
#15054 = AXIS2_PLACEMENT_3D('',#23451,#18807,#18808) ;
#15055 = AXIS2_PLACEMENT_3D('',#23457,#18812,#18813) ;
#15056 = AXIS2_PLACEMENT_3D('',#23463,#18817,#18818) ;
#15057 = AXIS2_PLACEMENT_3D('',#23469,#18822,#18823) ;
#15058 = AXIS2_PLACEMENT_3D('',#23470,#18824,#18825) ;
#15059 = AXIS2_PLACEMENT_3D('',#23472,#18827,#18828) ;
#15060 = AXIS2_PLACEMENT_3D('',#23473,#18829,#18830) ;
#15061 = AXIS2_PLACEMENT_3D('',#23476,#18831,#18832) ;
#15062 = AXIS2_PLACEMENT_3D('',#23482,#18836,#18837) ;
#15063 = AXIS2_PLACEMENT_3D('',#23488,#18841,#18842) ;
#15064 = AXIS2_PLACEMENT_3D('',#23494,#18846,#18847) ;
#15065 = AXIS2_PLACEMENT_3D('',#23495,#18848,#18849) ;
#15066 = AXIS2_PLACEMENT_3D('',#23497,#18851,#18852) ;
#15067 = AXIS2_PLACEMENT_3D('',#23498,#18853,#18854) ;
#15068 = AXIS2_PLACEMENT_3D('',#23501,#18855,#18856) ;
#15069 = AXIS2_PLACEMENT_3D('',#23507,#18860,#18861) ;
#15070 = AXIS2_PLACEMENT_3D('',#23513,#18865,#18866) ;
#15071 = AXIS2_PLACEMENT_3D('',#23519,#18870,#18871) ;
#15072 = AXIS2_PLACEMENT_3D('',#23520,#18872,#18873) ;
#15073 = AXIS2_PLACEMENT_3D('',#23522,#18875,#18876) ;
#15074 = AXIS2_PLACEMENT_3D('',#23523,#18877,#18878) ;
#15075 = AXIS2_PLACEMENT_3D('',#23526,#18879,#18880) ;
#15076 = AXIS2_PLACEMENT_3D('',#23532,#18884,#18885) ;
#15077 = AXIS2_PLACEMENT_3D('',#23538,#18889,#18890) ;
#15078 = AXIS2_PLACEMENT_3D('',#23544,#18894,#18895) ;
#15079 = AXIS2_PLACEMENT_3D('',#23545,#18896,#18897) ;
#15080 = AXIS2_PLACEMENT_3D('',#23547,#18899,#18900) ;
#15081 = AXIS2_PLACEMENT_3D('',#23548,#18901,#18902) ;
#15082 = AXIS2_PLACEMENT_3D('',#23551,#18903,#18904) ;
#15083 = AXIS2_PLACEMENT_3D('',#23557,#18908,#18909) ;
#15084 = AXIS2_PLACEMENT_3D('',#23563,#18913,#18914) ;
#15085 = AXIS2_PLACEMENT_3D('',#23569,#18918,#18919) ;
#15086 = AXIS2_PLACEMENT_3D('',#23570,#18920,#18921) ;
#15087 = AXIS2_PLACEMENT_3D('',#23572,#18923,#18924) ;
#15088 = AXIS2_PLACEMENT_3D('',#23573,#18925,#18926) ;
#15089 = AXIS2_PLACEMENT_3D('',#23575,#18927,#18928) ;
#15090 = AXIS2_PLACEMENT_3D('',#23579,#18931,#18932) ;
#15091 = AXIS2_PLACEMENT_3D('',#23580,#18933,#18934) ;
#15092 = AXIS2_PLACEMENT_3D('',#23581,#18935,#18936) ;
#15093 = AXIS2_PLACEMENT_3D('',#23582,#18937,#18938) ;
#15094 = AXIS2_PLACEMENT_3D('',#23583,#18939,#18940) ;
#15095 = AXIS2_PLACEMENT_3D('',#23585,#18941,#18942) ;
#15096 = AXIS2_PLACEMENT_3D('',#23588,#18944,#18945) ;
#15097 = AXIS2_PLACEMENT_3D('',#23589,#18946,#18947) ;
#15098 = AXIS2_PLACEMENT_3D('',#23591,#18948,#18949) ;
#15099 = AXIS2_PLACEMENT_3D('',#23594,#18951,#18952) ;
#15100 = AXIS2_PLACEMENT_3D('',#23595,#18953,#18954) ;
#15101 = AXIS2_PLACEMENT_3D('',#23596,#18955,#18956) ;
#15102 = AXIS2_PLACEMENT_3D('',#23597,#18957,#18958) ;
#15103 = AXIS2_PLACEMENT_3D('',#23598,#18959,#18960) ;
#15104 = AXIS2_PLACEMENT_3D('',#23603,#18962,#18963) ;
#15105 = AXIS2_PLACEMENT_3D('',#23606,#18965,#18966) ;
#15106 = AXIS2_PLACEMENT_3D('',#23607,#18967,#18968) ;
#15107 = AXIS2_PLACEMENT_3D('',#23609,#18969,#18970) ;
#15108 = AXIS2_PLACEMENT_3D('',#23611,#18972,#18973) ;
#15109 = AXIS2_PLACEMENT_3D('',#23612,#18974,#18975) ;
#15110 = AXIS2_PLACEMENT_3D('',#23619,#18979,#18980) ;
#15111 = AXIS2_PLACEMENT_3D('',#23650,#18981,#18982) ;
#15112 = AXIS2_PLACEMENT_3D('',#23651,#18983,#18984) ;
#15113 = AXIS2_PLACEMENT_3D('',#23652,#18985,#18986) ;
#15114 = AXIS2_PLACEMENT_3D('',#23656,#18988,#18989) ;
#15115 = AXIS2_PLACEMENT_3D('',#23658,#18990,#18991) ;
#15116 = AXIS2_PLACEMENT_3D('',#23659,#18992,#18993) ;
#15117 = AXIS2_PLACEMENT_3D('',#23660,#18994,#18995) ;
#15118 = AXIS2_PLACEMENT_3D('',#23661,#18996,#18997) ;
#15119 = AXIS2_PLACEMENT_3D('',#23662,#18998,#18999) ;
#15120 = AXIS2_PLACEMENT_3D('',#23664,#19000,#19001) ;
#15121 = AXIS2_PLACEMENT_3D('',#23665,#19002,#19003) ;
#15122 = AXIS2_PLACEMENT_3D('',#23666,#19004,#19005) ;
#15123 = AXIS2_PLACEMENT_3D('',#23667,#19006,#19007) ;
#15124 = AXIS2_PLACEMENT_3D('',#23670,#19008,#19009) ;
#15125 = AXIS2_PLACEMENT_3D('',#23672,#19010,#19011) ;
#15126 = AXIS2_PLACEMENT_3D('',#23674,#19012,#19013) ;
#15127 = AXIS2_PLACEMENT_3D('',#23676,#19014,#19015) ;
#15128 = AXIS2_PLACEMENT_3D('',#23677,#19016,#19017) ;
#15129 = AXIS2_PLACEMENT_3D('',#23678,#19018,#19019) ;
#15130 = AXIS2_PLACEMENT_3D('',#23681,#19020,#19021) ;
#15131 = AXIS2_PLACEMENT_3D('',#23682,#19022,#19023) ;
#15132 = AXIS2_PLACEMENT_3D('',#23683,#19024,#19025) ;
#15133 = AXIS2_PLACEMENT_3D('',#23684,#19026,#19027) ;
#15134 = AXIS2_PLACEMENT_3D('',#23687,#19029,#19030) ;
#15135 = AXIS2_PLACEMENT_3D('',#23688,#19031,#19032) ;
#15136 = AXIS2_PLACEMENT_3D('',#23689,#19033,#19034) ;
#15137 = AXIS2_PLACEMENT_3D('',#23691,#19036,#19037) ;
#15138 = AXIS2_PLACEMENT_3D('',#23692,#19038,#19039) ;
#15139 = AXIS2_PLACEMENT_3D('',#23695,#19041,#19042) ;
#15140 = AXIS2_PLACEMENT_3D('',#23696,#19043,#19044) ;
#15141 = AXIS2_PLACEMENT_3D('',#23698,#19045,#19046) ;
#15142 = AXIS2_PLACEMENT_3D('',#23700,#19048,#19049) ;
#15143 = AXIS2_PLACEMENT_3D('',#23701,#19050,#19051) ;
#15144 = AXIS2_PLACEMENT_3D('',#23702,#19052,#19053) ;
#15145 = AXIS2_PLACEMENT_3D('',#23711,#19058,#19059) ;
#15146 = AXIS2_PLACEMENT_3D('',#23720,#19064,#19065) ;
#15147 = AXIS2_PLACEMENT_3D('',#23729,#19070,#19071) ;
#15148 = AXIS2_PLACEMENT_3D('',#23732,#19074,#19075) ;
#15149 = AXIS2_PLACEMENT_3D('',#23733,#19076,#19077) ;
#15150 = AXIS2_PLACEMENT_3D('',#23734,#19078,#19079) ;
#15151 = AXIS2_PLACEMENT_3D('',#23735,#19080,#19081) ;
#15152 = AXIS2_PLACEMENT_3D('',#23736,#19082,#19083) ;
#15153 = AXIS2_PLACEMENT_3D('',#23737,#19084,#19085) ;
#15154 = AXIS2_PLACEMENT_3D('',#23738,#19086,#19087) ;
#15155 = AXIS2_PLACEMENT_3D('',#23739,#19088,#19089) ;
#15156 = AXIS2_PLACEMENT_3D('',#23740,#19090,#19091) ;
#15157 = AXIS2_PLACEMENT_3D('',#23741,#19092,#19093) ;
#15158 = AXIS2_PLACEMENT_3D('',#23750,#19098,#19099) ;
#15159 = AXIS2_PLACEMENT_3D('',#23759,#19104,#19105) ;
#15160 = AXIS2_PLACEMENT_3D('',#23768,#19110,#19111) ;
#15161 = AXIS2_PLACEMENT_3D('',#23771,#19114,#19115) ;
#15162 = AXIS2_PLACEMENT_3D('',#23772,#19116,#19117) ;
#15163 = AXIS2_PLACEMENT_3D('',#23773,#19118,#19119) ;
#15164 = AXIS2_PLACEMENT_3D('',#23774,#19120,#19121) ;
#15165 = AXIS2_PLACEMENT_3D('',#23775,#19122,#19123) ;
#15166 = AXIS2_PLACEMENT_3D('',#23776,#19124,#19125) ;
#15167 = AXIS2_PLACEMENT_3D('',#23777,#19126,#19127) ;
#15168 = AXIS2_PLACEMENT_3D('',#23778,#19128,#19129) ;
#15169 = AXIS2_PLACEMENT_3D('',#23779,#19130,#19131) ;
#15170 = AXIS2_PLACEMENT_3D('',#23780,#19132,#19133) ;
#15171 = AXIS2_PLACEMENT_3D('',#23781,#19134,#19135) ;
#15172 = AXIS2_PLACEMENT_3D('',#23782,#19136,#19137) ;
#15173 = AXIS2_PLACEMENT_3D('',#23783,#19138,#19139) ;
#15174 = AXIS2_PLACEMENT_3D('',#23784,#19140,#19141) ;
#15175 = AXIS2_PLACEMENT_3D('',#23785,#19142,#19143) ;
#15176 = AXIS2_PLACEMENT_3D('',#23786,#19144,#19145) ;
#15177 = AXIS2_PLACEMENT_3D('',#23787,#19146,#19147) ;
#15178 = AXIS2_PLACEMENT_3D('',#23788,#19148,#19149) ;
#15179 = AXIS2_PLACEMENT_3D('',#23789,#19150,#19151) ;
#15180 = AXIS2_PLACEMENT_3D('',#23790,#19152,#19153) ;
#15181 = AXIS2_PLACEMENT_3D('',#23791,#19154,#19155) ;
#15182 = AXIS2_PLACEMENT_3D('',#23792,#19156,#19157) ;
#15183 = AXIS2_PLACEMENT_3D('',#23793,#19158,#19159) ;
#15184 = AXIS2_PLACEMENT_3D('',#23909,#19161,#19162) ;
#15185 = AXIS2_PLACEMENT_3D('',#23911,#19163,#19164) ;
#15186 = AXIS2_PLACEMENT_3D('',#23915,#19167,#19168) ;
#15187 = AXIS2_PLACEMENT_3D('',#23916,#19169,#19170) ;
#15188 = AXIS2_PLACEMENT_3D('',#23918,#19171,#19172) ;
#15189 = AXIS2_PLACEMENT_3D('',#23922,#19175,#19176) ;
#15190 = AXIS2_PLACEMENT_3D('',#23923,#19177,#19178) ;
#15191 = AXIS2_PLACEMENT_3D('',#23924,#19179,#19180) ;
#15192 = AXIS2_PLACEMENT_3D('',#23925,#19181,#19182) ;
#15193 = AXIS2_PLACEMENT_3D('',#23926,#19183,#19184) ;
#15194 = AXIS2_PLACEMENT_3D('',#23931,#19186,#19187) ;
#15195 = AXIS2_PLACEMENT_3D('',#23934,#19189,#19190) ;
#15196 = AXIS2_PLACEMENT_3D('',#23935,#19191,#19192) ;
#15197 = AXIS2_PLACEMENT_3D('',#23986,#19193,#19194) ;
#15198 = AXIS2_PLACEMENT_3D('',#23999,#19195,#19196) ;
#15199 = AXIS2_PLACEMENT_3D('',#24015,#19197,#19198) ;
#15200 = AXIS2_PLACEMENT_3D('',#24063,#19199,#19200) ;
#15201 = AXIS2_PLACEMENT_3D('',#24066,#19203,#19204) ;
#15202 = AXIS2_PLACEMENT_3D('',#24068,#19205,#19206) ;
#15203 = AXIS2_PLACEMENT_3D('',#24072,#19209,#19210) ;
#15204 = AXIS2_PLACEMENT_3D('',#24073,#19211,#19212) ;
#15205 = AXIS2_PLACEMENT_3D('',#24075,#19213,#19214) ;
#15206 = AXIS2_PLACEMENT_3D('',#24078,#19216,#19217) ;
#15207 = AXIS2_PLACEMENT_3D('',#24079,#19218,#19219) ;
#15208 = AXIS2_PLACEMENT_3D('',#24080,#19220,#19221) ;
#15209 = AXIS2_PLACEMENT_3D('',#24084,#19224,#19225) ;
#15210 = AXIS2_PLACEMENT_3D('',#24085,#19226,#19227) ;
#15211 = AXIS2_PLACEMENT_3D('',#24088,#19229,#19230) ;
#15212 = AXIS2_PLACEMENT_3D('',#24089,#19231,#19232) ;
#15213 = AXIS2_PLACEMENT_3D('',#24090,#19233,#19234) ;
#15214 = AXIS2_PLACEMENT_3D('',#24091,#19235,#19236) ;
#15215 = AXIS2_PLACEMENT_3D('',#24093,#19237,#19238) ;
#15216 = AXIS2_PLACEMENT_3D('',#24096,#19240,#19241) ;
#15217 = AXIS2_PLACEMENT_3D('',#24097,#19242,#19243) ;
#15218 = AXIS2_PLACEMENT_3D('',#24099,#19244,#19245) ;
#15219 = AXIS2_PLACEMENT_3D('',#24102,#19247,#19248) ;
#15220 = AXIS2_PLACEMENT_3D('',#24103,#19249,#19250) ;
#15221 = AXIS2_PLACEMENT_3D('',#24104,#19251,#19252) ;
#15222 = AXIS2_PLACEMENT_3D('',#24105,#19253,#19254) ;
#15223 = AXIS2_PLACEMENT_3D('',#24106,#19255,#19256) ;
#15224 = AXIS2_PLACEMENT_3D('',#24108,#19257,#19258) ;
#15225 = AXIS2_PLACEMENT_3D('',#24111,#19260,#19261) ;
#15226 = AXIS2_PLACEMENT_3D('',#24112,#19262,#19263) ;
#15227 = AXIS2_PLACEMENT_3D('',#24114,#19264,#19265) ;
#15228 = AXIS2_PLACEMENT_3D('',#24117,#19267,#19268) ;
#15229 = AXIS2_PLACEMENT_3D('',#24118,#19269,#19270) ;
#15230 = AXIS2_PLACEMENT_3D('',#24120,#19271,#19272) ;
#15231 = AXIS2_PLACEMENT_3D('',#24123,#19274,#19275) ;
#15232 = AXIS2_PLACEMENT_3D('',#24124,#19276,#19277) ;
#15233 = AXIS2_PLACEMENT_3D('',#24126,#19278,#19279) ;
#15234 = AXIS2_PLACEMENT_3D('',#24129,#19281,#19282) ;
#15235 = AXIS2_PLACEMENT_3D('',#24130,#19283,#19284) ;
#15236 = AXIS2_PLACEMENT_3D('',#24132,#19285,#19286) ;
#15237 = AXIS2_PLACEMENT_3D('',#24135,#19288,#19289) ;
#15238 = AXIS2_PLACEMENT_3D('',#24136,#19290,#19291) ;
#15239 = AXIS2_PLACEMENT_3D('',#24138,#19292,#19293) ;
#15240 = AXIS2_PLACEMENT_3D('',#24141,#19295,#19296) ;
#15241 = AXIS2_PLACEMENT_3D('',#24142,#19297,#19298) ;
#15242 = AXIS2_PLACEMENT_3D('',#24143,#19299,#19300) ;
#15243 = AXIS2_PLACEMENT_3D('',#24144,#19301,#19302) ;
#15244 = AXIS2_PLACEMENT_3D('',#24145,#19303,#19304) ;
#15245 = AXIS2_PLACEMENT_3D('',#24147,#19305,#19306) ;
#15246 = AXIS2_PLACEMENT_3D('',#24150,#19308,#19309) ;
#15247 = AXIS2_PLACEMENT_3D('',#24151,#19310,#19311) ;
#15248 = AXIS2_PLACEMENT_3D('',#24153,#19312,#19313) ;
#15249 = AXIS2_PLACEMENT_3D('',#24156,#19315,#19316) ;
#15250 = AXIS2_PLACEMENT_3D('',#24157,#19317,#19318) ;
#15251 = AXIS2_PLACEMENT_3D('',#24159,#19319,#19320) ;
#15252 = AXIS2_PLACEMENT_3D('',#24162,#19322,#19323) ;
#15253 = AXIS2_PLACEMENT_3D('',#24163,#19324,#19325) ;
#15254 = AXIS2_PLACEMENT_3D('',#24165,#19326,#19327) ;
#15255 = AXIS2_PLACEMENT_3D('',#24168,#19329,#19330) ;
#15256 = AXIS2_PLACEMENT_3D('',#24169,#19331,#19332) ;
#15257 = AXIS2_PLACEMENT_3D('',#24171,#19333,#19334) ;
#15258 = AXIS2_PLACEMENT_3D('',#24174,#19336,#19337) ;
#15259 = AXIS2_PLACEMENT_3D('',#24175,#19338,#19339) ;
#15260 = AXIS2_PLACEMENT_3D('',#24177,#19340,#19341) ;
#15261 = AXIS2_PLACEMENT_3D('',#24180,#19343,#19344) ;
#15262 = AXIS2_PLACEMENT_3D('',#24181,#19345,#19346) ;
#15263 = AXIS2_PLACEMENT_3D('',#24182,#19347,#19348) ;
#15264 = AXIS2_PLACEMENT_3D('',#24183,#19349,#19350) ;
#15265 = AXIS2_PLACEMENT_3D('',#24184,#19351,#19352) ;
#15266 = AXIS2_PLACEMENT_3D('',#24188,#19354,#19355) ;
#15267 = AXIS2_PLACEMENT_3D('',#24189,#19356,#19357) ;
#15268 = AXIS2_PLACEMENT_3D('',#24191,#19358,#19359) ;
#15269 = AXIS2_PLACEMENT_3D('',#24194,#19361,#19362) ;
#15270 = AXIS2_PLACEMENT_3D('',#24195,#19363,#19364) ;
#15271 = AXIS2_PLACEMENT_3D('',#24215,#19365,#19366) ;
#15272 = AXIS2_PLACEMENT_3D('',#24219,#19368,#19369) ;
#15273 = AXIS2_PLACEMENT_3D('',#24220,#19370,#19371) ;
#15274 = AXIS2_PLACEMENT_3D('',#24222,#19372,#19373) ;
#15275 = AXIS2_PLACEMENT_3D('',#24225,#19375,#19376) ;
#15276 = AXIS2_PLACEMENT_3D('',#24226,#19377,#19378) ;
#15277 = AXIS2_PLACEMENT_3D('',#24245,#19379,#19380) ;
#15278 = AXIS2_PLACEMENT_3D('',#24254,#19385,#19386) ;
#15279 = AXIS2_PLACEMENT_3D('',#24263,#19391,#19392) ;
#15280 = AXIS2_PLACEMENT_3D('',#24272,#19397,#19398) ;
#15281 = AXIS2_PLACEMENT_3D('',#24275,#19401,#19402) ;
#15282 = AXIS2_PLACEMENT_3D('',#24278,#19405,#19406) ;
#15283 = AXIS2_PLACEMENT_3D('',#24279,#19407,#19408) ;
#15284 = AXIS2_PLACEMENT_3D('',#24281,#19409,#19410) ;
#15285 = AXIS2_PLACEMENT_3D('',#24282,#19411,#19412) ;
#15286 = AXIS2_PLACEMENT_3D('',#24283,#19413,#19414) ;
#15287 = AXIS2_PLACEMENT_3D('',#24284,#19415,#19416) ;
#15288 = AXIS2_PLACEMENT_3D('',#24287,#19418,#19419) ;
#15289 = AXIS2_PLACEMENT_3D('',#24288,#19420,#19421) ;
#15290 = AXIS2_PLACEMENT_3D('',#24289,#19422,#19423) ;
#15291 = AXIS2_PLACEMENT_3D('',#24290,#19424,#19425) ;
#15292 = AXIS2_PLACEMENT_3D('',#24291,#19426,#19427) ;
#15293 = AXIS2_PLACEMENT_3D('',#24292,#19428,#19429) ;
#15294 = AXIS2_PLACEMENT_3D('',#24293,#19430,#19431) ;
#15295 = AXIS2_PLACEMENT_3D('',#24294,#19432,#19433) ;
#15296 = AXIS2_PLACEMENT_3D('',#24295,#19434,#19435) ;
#15297 = AXIS2_PLACEMENT_3D('',#24296,#19436,#19437) ;
#15298 = AXIS2_PLACEMENT_3D('',#24297,#19438,#19439) ;
#15299 = AXIS2_PLACEMENT_3D('',#24298,#19440,#19441) ;
#15300 = AXIS2_PLACEMENT_3D('',#24300,#19442,#19443) ;
#15301 = AXIS2_PLACEMENT_3D('',#24303,#19445,#19446) ;
#15302 = AXIS2_PLACEMENT_3D('',#24304,#19447,#19448) ;
#15303 = AXIS2_PLACEMENT_3D('',#24305,#19449,#19450) ;
#15304 = AXIS2_PLACEMENT_3D('',#24307,#19451,#19452) ;
#15305 = AXIS2_PLACEMENT_3D('',#24310,#19454,#19455) ;
#15306 = AXIS2_PLACEMENT_3D('',#24311,#19456,#19457) ;
#15307 = AXIS2_PLACEMENT_3D('',#24312,#19458,#19459) ;
#15308 = AXIS2_PLACEMENT_3D('',#24313,#19460,#19461) ;
#15309 = AXIS2_PLACEMENT_3D('',#24314,#19462,#19463) ;
#15310 = AXIS2_PLACEMENT_3D('',#24316,#19464,#19465) ;
#15311 = AXIS2_PLACEMENT_3D('',#24319,#19467,#19468) ;
#15312 = AXIS2_PLACEMENT_3D('',#24320,#19469,#19470) ;
#15313 = AXIS2_PLACEMENT_3D('',#24322,#19471,#19472) ;
#15314 = AXIS2_PLACEMENT_3D('',#24325,#19474,#19475) ;
#15315 = AXIS2_PLACEMENT_3D('',#24326,#19476,#19477) ;
#15316 = AXIS2_PLACEMENT_3D('',#24327,#19478,#19479) ;
#15317 = AXIS2_PLACEMENT_3D('',#24328,#19480,#19481) ;
#15318 = AXIS2_PLACEMENT_3D('',#24329,#19482,#19483) ;
#15319 = AXIS2_PLACEMENT_3D('',#24331,#19484,#19485) ;
#15320 = AXIS2_PLACEMENT_3D('',#24334,#19487,#19488) ;
#15321 = AXIS2_PLACEMENT_3D('',#24335,#19489,#19490) ;
#15322 = AXIS2_PLACEMENT_3D('',#24344,#19495,#19496) ;
#15323 = AXIS2_PLACEMENT_3D('',#24353,#19501,#19502) ;
#15324 = AXIS2_PLACEMENT_3D('',#24360,#19507,#19508) ;
#15325 = AXIS2_PLACEMENT_3D('',#24364,#19511,#19512) ;
#15326 = AXIS2_PLACEMENT_3D('',#24368,#19515,#19516) ;
#15327 = AXIS2_PLACEMENT_3D('',#24370,#19518,#19519) ;
#15328 = AXIS2_PLACEMENT_3D('',#24372,#19521,#19522) ;
#15329 = AXIS2_PLACEMENT_3D('',#24373,#19523,#19524) ;
#15330 = AXIS2_PLACEMENT_3D('',#24374,#19525,#19526) ;
#15331 = AXIS2_PLACEMENT_3D('',#24376,#19527,#19528) ;
#15332 = AXIS2_PLACEMENT_3D('',#24379,#19530,#19531) ;
#15333 = AXIS2_PLACEMENT_3D('',#24380,#19532,#19533) ;
#15334 = AXIS2_PLACEMENT_3D('',#24381,#19534,#19535) ;
#15335 = AXIS2_PLACEMENT_3D('',#24390,#19540,#19541) ;
#15336 = AXIS2_PLACEMENT_3D('',#24399,#19546,#19547) ;
#15337 = AXIS2_PLACEMENT_3D('',#24406,#19552,#19553) ;
#15338 = AXIS2_PLACEMENT_3D('',#24410,#19556,#19557) ;
#15339 = AXIS2_PLACEMENT_3D('',#24414,#19560,#19561) ;
#15340 = AXIS2_PLACEMENT_3D('',#24416,#19563,#19564) ;
#15341 = AXIS2_PLACEMENT_3D('',#24418,#19566,#19567) ;
#15342 = AXIS2_PLACEMENT_3D('',#24419,#19568,#19569) ;
#15343 = AXIS2_PLACEMENT_3D('',#24420,#19570,#19571) ;
#15344 = AXIS2_PLACEMENT_3D('',#24422,#19572,#19573) ;
#15345 = AXIS2_PLACEMENT_3D('',#24425,#19575,#19576) ;
#15346 = AXIS2_PLACEMENT_3D('',#24426,#19577,#19578) ;
#15347 = AXIS2_PLACEMENT_3D('',#24427,#19579,#19580) ;
#15348 = AXIS2_PLACEMENT_3D('',#24436,#19585,#19586) ;
#15349 = AXIS2_PLACEMENT_3D('',#24445,#19591,#19592) ;
#15350 = AXIS2_PLACEMENT_3D('',#24452,#19597,#19598) ;
#15351 = AXIS2_PLACEMENT_3D('',#24456,#19601,#19602) ;
#15352 = AXIS2_PLACEMENT_3D('',#24460,#19605,#19606) ;
#15353 = AXIS2_PLACEMENT_3D('',#24462,#19608,#19609) ;
#15354 = AXIS2_PLACEMENT_3D('',#24464,#19611,#19612) ;
#15355 = AXIS2_PLACEMENT_3D('',#24465,#19613,#19614) ;
#15356 = AXIS2_PLACEMENT_3D('',#24466,#19615,#19616) ;
#15357 = AXIS2_PLACEMENT_3D('',#24468,#19617,#19618) ;
#15358 = AXIS2_PLACEMENT_3D('',#24471,#19620,#19621) ;
#15359 = AXIS2_PLACEMENT_3D('',#24472,#19622,#19623) ;
#15360 = AXIS2_PLACEMENT_3D('',#24481,#19628,#19629) ;
#15361 = AXIS2_PLACEMENT_3D('',#24490,#19634,#19635) ;
#15362 = AXIS2_PLACEMENT_3D('',#24497,#19640,#19641) ;
#15363 = AXIS2_PLACEMENT_3D('',#24501,#19644,#19645) ;
#15364 = AXIS2_PLACEMENT_3D('',#24505,#19648,#19649) ;
#15365 = AXIS2_PLACEMENT_3D('',#24507,#19651,#19652) ;
#15366 = AXIS2_PLACEMENT_3D('',#24509,#19654,#19655) ;
#15367 = AXIS2_PLACEMENT_3D('',#24510,#19656,#19657) ;
#15368 = AXIS2_PLACEMENT_3D('',#24511,#19658,#19659) ;
#15369 = AXIS2_PLACEMENT_3D('',#24512,#19660,#19661) ;
#15370 = AXIS2_PLACEMENT_3D('',#24513,#19662,#19663) ;
#15371 = AXIS2_PLACEMENT_3D('',#24514,#19664,#19665) ;
#15372 = AXIS2_PLACEMENT_3D('',#24515,#19666,#19667) ;
#15373 = AXIS2_PLACEMENT_3D('',#24516,#19668,#19669) ;
#15374 = AXIS2_PLACEMENT_3D('',#24517,#19670,#19671) ;
#15375 = AXIS2_PLACEMENT_3D('',#24518,#19672,#19673) ;
#15376 = AXIS2_PLACEMENT_3D('',#24519,#19674,#19675) ;
#15377 = AXIS2_PLACEMENT_3D('',#24520,#19676,#19677) ;
#15378 = AXIS2_PLACEMENT_3D('',#24521,#19678,#19679) ;
#15379 = AXIS2_PLACEMENT_3D('',#24522,#19680,#19681) ;
#15380 = AXIS2_PLACEMENT_3D('',#24523,#19682,#19683) ;
#15381 = AXIS2_PLACEMENT_3D('',#24524,#19684,#19685) ;
#15382 = AXIS2_PLACEMENT_3D('',#24525,#19686,#19687) ;
#15383 = AXIS2_PLACEMENT_3D('',#24526,#19688,#19689) ;
#15384 = AXIS2_PLACEMENT_3D('',#24527,#19690,#19691) ;
#15385 = AXIS2_PLACEMENT_3D('',#24528,#19692,#19693) ;
#15386 = AXIS2_PLACEMENT_3D('',#24529,#19694,#19695) ;
#15387 = AXIS2_PLACEMENT_3D('',#24530,#19696,#19697) ;
#15388 = AXIS2_PLACEMENT_3D('',#24531,#19698,#19699) ;
#15389 = AXIS2_PLACEMENT_3D('',#24532,#19700,#19701) ;
#15390 = DIRECTION('axis',(0.,0.,1.)) ;
#15391 = DIRECTION('refdir',(1.,0.,0.)) ;
#15392 = DIRECTION('axis',(0.,0.,1.)) ;
#15393 = DIRECTION('refdir',(1.,0.,0.)) ;
#15394 = DIRECTION('axis',(0.,0.,1.)) ;
#15395 = DIRECTION('refdir',(1.,0.,0.)) ;
#15396 = DIRECTION('center_axis',(0.,1.,0.)) ;
#15397 = DIRECTION('ref_axis',(1.,0.,0.)) ;
#15398 = DIRECTION('center_axis',(0.,-1.,0.)) ;
#15399 = DIRECTION('ref_axis',(1.,0.,0.)) ;
#15400 = DIRECTION('center_axis',(0.,1.,0.)) ;
#15401 = DIRECTION('ref_axis',(1.,0.,0.)) ;
#15402 = DIRECTION('center_axis',(0.,1.,0.)) ;
#15403 = DIRECTION('ref_axis',(1.,0.,0.)) ;
#15404 = DIRECTION('center_axis',(0.,1.,0.)) ;
#15405 = DIRECTION('ref_axis',(1.,0.,0.)) ;
#15406 = DIRECTION('center_axis',(0.,1.,0.)) ;
#15407 = DIRECTION('ref_axis',(1.,0.,0.)) ;
#15408 = DIRECTION('',(0.,1.,0.)) ;
#15409 = DIRECTION('',(0.,1.,0.)) ;
#15410 = DIRECTION('center_axis',(0.,-1.,0.)) ;
#15411 = DIRECTION('ref_axis',(1.,0.,0.)) ;
#15412 = DIRECTION('',(0.,-1.,0.)) ;
#15413 = DIRECTION('center_axis',(0.,1.,0.)) ;
#15414 = DIRECTION('ref_axis',(1.,0.,0.)) ;
#15415 = DIRECTION('center_axis',(0.,-1.,0.)) ;
#15416 = DIRECTION('ref_axis',(1.,0.,0.)) ;
#15417 = DIRECTION('',(0.,1.,0.)) ;
#15418 = DIRECTION('center_axis',(0.,-1.,0.)) ;
#15419 = DIRECTION('ref_axis',(1.,0.,0.)) ;
#15420 = DIRECTION('',(0.,-1.,0.)) ;
#15421 = DIRECTION('center_axis',(0.,-1.,0.)) ;
#15422 = DIRECTION('ref_axis',(1.,0.,0.)) ;
#15423 = DIRECTION('',(0.,1.,0.)) ;
#15424 = DIRECTION('center_axis',(0.,-1.,0.)) ;
#15425 = DIRECTION('ref_axis',(1.,0.,0.)) ;
#15426 = DIRECTION('center_axis',(0.,-1.,0.)) ;
#15427 = DIRECTION('ref_axis',(1.,0.,0.)) ;
#15428 = DIRECTION('',(0.,1.,0.)) ;
#15429 = DIRECTION('center_axis',(0.,-1.,0.)) ;
#15430 = DIRECTION('ref_axis',(1.,0.,0.)) ;
#15431 = DIRECTION('',(0.,-1.,0.)) ;
#15432 = DIRECTION('center_axis',(0.,-1.,0.)) ;
#15433 = DIRECTION('ref_axis',(1.,0.,0.)) ;
#15434 = DIRECTION('',(0.,1.,0.)) ;
#15435 = DIRECTION('',(0.,1.,0.)) ;
#15436 = DIRECTION('center_axis',(0.,1.,0.)) ;
#15437 = DIRECTION('ref_axis',(1.,0.,0.)) ;
#15438 = DIRECTION('center_axis',(0.,1.,0.)) ;
#15439 = DIRECTION('ref_axis',(1.,0.,0.)) ;
#15440 = DIRECTION('',(0.,1.,0.)) ;
#15441 = DIRECTION('center_axis',(0.,1.,0.)) ;
#15442 = DIRECTION('ref_axis',(1.,0.,0.)) ;
#15443 = DIRECTION('center_axis',(0.,-1.,0.)) ;
#15444 = DIRECTION('ref_axis',(1.,0.,0.)) ;
#15445 = DIRECTION('center_axis',(0.,1.,0.)) ;
#15446 = DIRECTION('ref_axis',(1.,0.,0.)) ;
#15447 = DIRECTION('center_axis',(0.,1.,0.)) ;
#15448 = DIRECTION('ref_axis',(1.,0.,0.)) ;
#15449 = DIRECTION('center_axis',(0.,-1.,0.)) ;
#15450 = DIRECTION('ref_axis',(-1.,0.,0.)) ;
#15451 = DIRECTION('center_axis',(0.,-1.,0.)) ;
#15452 = DIRECTION('ref_axis',(1.,0.,0.)) ;
#15453 = DIRECTION('center_axis',(0.,-1.,0.)) ;
#15454 = DIRECTION('ref_axis',(1.,0.,0.)) ;
#15455 = DIRECTION('center_axis',(0.,-1.,0.)) ;
#15456 = DIRECTION('ref_axis',(1.,0.,0.)) ;
#15457 = DIRECTION('center_axis',(0.,1.,0.)) ;
#15458 = DIRECTION('ref_axis',(1.,0.,0.)) ;
#15459 = DIRECTION('center_axis',(0.,1.,0.)) ;
#15460 = DIRECTION('ref_axis',(1.,0.,0.)) ;
#15461 = DIRECTION('',(0.,1.,0.)) ;
#15462 = DIRECTION('center_axis',(0.,-1.,0.)) ;
#15463 = DIRECTION('ref_axis',(1.,0.,0.)) ;
#15464 = DIRECTION('center_axis',(0.,1.,0.)) ;
#15465 = DIRECTION('ref_axis',(1.,0.,0.)) ;
#15466 = DIRECTION('center_axis',(0.,1.,0.)) ;
#15467 = DIRECTION('ref_axis',(1.,0.,0.)) ;
#15468 = DIRECTION('',(0.,1.,0.)) ;
#15469 = DIRECTION('center_axis',(0.,-1.,0.)) ;
#15470 = DIRECTION('ref_axis',(1.,0.,0.)) ;
#15471 = DIRECTION('center_axis',(0.,1.,0.)) ;
#15472 = DIRECTION('ref_axis',(1.,0.,0.)) ;
#15473 = DIRECTION('center_axis',(0.,1.,0.)) ;
#15474 = DIRECTION('ref_axis',(1.,0.,0.)) ;
#15475 = DIRECTION('',(0.,1.,0.)) ;
#15476 = DIRECTION('center_axis',(0.,-1.,0.)) ;
#15477 = DIRECTION('ref_axis',(1.,0.,0.)) ;
#15478 = DIRECTION('center_axis',(0.,1.,0.)) ;
#15479 = DIRECTION('ref_axis',(1.,0.,0.)) ;
#15480 = DIRECTION('center_axis',(0.,1.,0.)) ;
#15481 = DIRECTION('ref_axis',(1.,0.,0.)) ;
#15482 = DIRECTION('',(0.,1.,0.)) ;
#15483 = DIRECTION('center_axis',(0.,-1.,0.)) ;
#15484 = DIRECTION('ref_axis',(1.,0.,0.)) ;
#15485 = DIRECTION('center_axis',(0.,1.,0.)) ;
#15486 = DIRECTION('ref_axis',(1.,0.,0.)) ;
#15487 = DIRECTION('center_axis',(0.,1.,0.)) ;
#15488 = DIRECTION('ref_axis',(1.,0.,0.)) ;
#15489 = DIRECTION('',(0.,1.,0.)) ;
#15490 = DIRECTION('center_axis',(0.,-1.,0.)) ;
#15491 = DIRECTION('ref_axis',(1.,0.,0.)) ;
#15492 = DIRECTION('center_axis',(0.,1.,0.)) ;
#15493 = DIRECTION('ref_axis',(1.,0.,0.)) ;
#15494 = DIRECTION('center_axis',(0.,1.,0.)) ;
#15495 = DIRECTION('ref_axis',(1.,0.,0.)) ;
#15496 = DIRECTION('',(0.,1.,0.)) ;
#15497 = DIRECTION('center_axis',(0.,-1.,0.)) ;
#15498 = DIRECTION('ref_axis',(1.,0.,0.)) ;
#15499 = DIRECTION('center_axis',(1.,0.,0.)) ;
#15500 = DIRECTION('ref_axis',(0.,0.,-1.)) ;
#15501 = DIRECTION('',(0.,1.,0.)) ;
#15502 = DIRECTION('',(0.,0.,1.)) ;
#15503 = DIRECTION('',(0.,1.,0.)) ;
#15504 = DIRECTION('',(0.,0.,-1.)) ;
#15505 = DIRECTION('',(0.,-1.,0.)) ;
#15506 = DIRECTION('',(0.,0.,-1.)) ;
#15507 = DIRECTION('center_axis',(0.,0.,1.)) ;
#15508 = DIRECTION('ref_axis',(1.,0.,0.)) ;
#15509 = DIRECTION('',(-1.,0.,0.)) ;
#15510 = DIRECTION('',(0.,-1.,0.)) ;
#15511 = DIRECTION('',(-1.,0.,0.)) ;
#15512 = DIRECTION('center_axis',(0.,-1.,0.)) ;
#15513 = DIRECTION('ref_axis',(0.,0.,-1.)) ;
#15514 = DIRECTION('center_axis',(0.,1.,0.)) ;
#15515 = DIRECTION('ref_axis',(1.,0.,0.)) ;
#15516 = DIRECTION('',(-1.,0.,0.)) ;
#15517 = DIRECTION('center_axis',(0.,0.,1.)) ;
#15518 = DIRECTION('ref_axis',(1.,0.,0.)) ;
#15519 = DIRECTION('',(0.,1.,0.)) ;
#15520 = DIRECTION('',(-1.,0.,0.)) ;
#15521 = DIRECTION('',(1.,0.,0.)) ;
#15522 = DIRECTION('center_axis',(0.,1.,0.)) ;
#15523 = DIRECTION('ref_axis',(0.,0.,1.)) ;
#15524 = DIRECTION('',(0.,0.,-1.)) ;
#15525 = DIRECTION('center_axis',(0.,-1.,0.)) ;
#15526 = DIRECTION('ref_axis',(0.,0.,-1.)) ;
#15527 = DIRECTION('center_axis',(0.,1.,0.)) ;
#15528 = DIRECTION('ref_axis',(1.,0.,0.)) ;
#15529 = DIRECTION('',(0.,0.,-1.)) ;
#15530 = DIRECTION('center_axis',(-1.,0.,0.)) ;
#15531 = DIRECTION('ref_axis',(0.,0.,1.)) ;
#15532 = DIRECTION('',(0.,-1.,0.)) ;
#15533 = DIRECTION('',(0.,0.,-1.)) ;
#15534 = DIRECTION('center_axis',(0.,1.,0.)) ;
#15535 = DIRECTION('ref_axis',(1.,0.,0.)) ;
#15536 = DIRECTION('center_axis',(0.,1.,0.)) ;
#15537 = DIRECTION('ref_axis',(1.,0.,0.)) ;
#15538 = DIRECTION('',(0.,-1.,0.)) ;
#15539 = DIRECTION('center_axis',(0.,-1.,0.)) ;
#15540 = DIRECTION('ref_axis',(1.,0.,0.)) ;
#15541 = DIRECTION('center_axis',(0.,-1.,0.)) ;
#15542 = DIRECTION('ref_axis',(1.,0.,0.)) ;
#15543 = DIRECTION('',(0.,1.,0.)) ;
#15544 = DIRECTION('center_axis',(0.,1.,0.)) ;
#15545 = DIRECTION('ref_axis',(1.,0.,0.)) ;
#15546 = DIRECTION('',(0.,-1.,0.)) ;
#15547 = DIRECTION('center_axis',(0.,-1.,0.)) ;
#15548 = DIRECTION('ref_axis',(1.,0.,0.)) ;
#15549 = DIRECTION('center_axis',(0.,0.,1.)) ;
#15550 = DIRECTION('ref_axis',(1.,0.,0.)) ;
#15551 = DIRECTION('center_axis',(0.,0.,1.)) ;
#15552 = DIRECTION('ref_axis',(1.,0.,0.)) ;
#15553 = DIRECTION('',(0.,0.,1.)) ;
#15554 = DIRECTION('center_axis',(0.,0.,-1.)) ;
#15555 = DIRECTION('ref_axis',(1.,0.,0.)) ;
#15556 = DIRECTION('center_axis',(0.,0.,1.)) ;
#15557 = DIRECTION('ref_axis',(1.,0.,0.)) ;
#15558 = DIRECTION('',(0.,0.,-1.)) ;
#15559 = DIRECTION('center_axis',(0.,0.,-1.)) ;
#15560 = DIRECTION('ref_axis',(1.,0.,0.)) ;
#15561 = DIRECTION('center_axis',(0.,0.,1.)) ;
#15562 = DIRECTION('ref_axis',(1.,0.,0.)) ;
#15563 = DIRECTION('center_axis',(0.,0.,1.)) ;
#15564 = DIRECTION('ref_axis',(1.,0.,0.)) ;
#15565 = DIRECTION('center_axis',(0.,0.,-1.)) ;
#15566 = DIRECTION('ref_axis',(-1.,0.,0.)) ;
#15567 = DIRECTION('center_axis',(0.,0.,1.)) ;
#15568 = DIRECTION('ref_axis',(1.,0.,0.)) ;
#15569 = DIRECTION('center_axis',(0.,1.,0.)) ;
#15570 = DIRECTION('ref_axis',(1.,0.,0.)) ;
#15571 = DIRECTION('center_axis',(0.,1.,0.)) ;
#15572 = DIRECTION('ref_axis',(1.,0.,0.)) ;
#15573 = DIRECTION('center_axis',(0.,1.,0.)) ;
#15574 = DIRECTION('ref_axis',(1.,0.,0.)) ;
#15575 = DIRECTION('center_axis',(0.,1.,0.)) ;
#15576 = DIRECTION('ref_axis',(1.,0.,0.)) ;
#15577 = DIRECTION('',(0.,1.,0.)) ;
#15578 = DIRECTION('center_axis',(0.,1.,0.)) ;
#15579 = DIRECTION('ref_axis',(1.,0.,0.)) ;
#15580 = DIRECTION('center_axis',(0.,1.,0.)) ;
#15581 = DIRECTION('ref_axis',(1.,0.,0.)) ;
#15582 = DIRECTION('center_axis',(0.,1.,0.)) ;
#15583 = DIRECTION('ref_axis',(1.,0.,0.)) ;
#15584 = DIRECTION('center_axis',(0.,1.,0.)) ;
#15585 = DIRECTION('ref_axis',(1.,0.,0.)) ;
#15586 = DIRECTION('',(0.,-1.,0.)) ;
#15587 = DIRECTION('center_axis',(0.,-1.,0.)) ;
#15588 = DIRECTION('ref_axis',(1.,0.,0.)) ;
#15589 = DIRECTION('center_axis',(0.,1.,0.)) ;
#15590 = DIRECTION('ref_axis',(1.,0.,0.)) ;
#15591 = DIRECTION('center_axis',(0.,-1.,0.)) ;
#15592 = DIRECTION('ref_axis',(-1.,0.,0.)) ;
#15593 = DIRECTION('center_axis',(0.,-1.,0.)) ;
#15594 = DIRECTION('ref_axis',(-1.,0.,0.)) ;
#15595 = DIRECTION('center_axis',(0.,1.,0.)) ;
#15596 = DIRECTION('ref_axis',(1.,0.,0.)) ;
#15597 = DIRECTION('center_axis',(0.,1.,0.)) ;
#15598 = DIRECTION('ref_axis',(1.,0.,0.)) ;
#15599 = DIRECTION('center_axis',(0.,1.,0.)) ;
#15600 = DIRECTION('ref_axis',(1.,0.,0.)) ;
#15601 = DIRECTION('',(0.,1.,0.)) ;
#15602 = DIRECTION('center_axis',(0.,-1.,0.)) ;
#15603 = DIRECTION('ref_axis',(1.,0.,0.)) ;
#15604 = DIRECTION('center_axis',(0.,1.,0.)) ;
#15605 = DIRECTION('ref_axis',(1.,0.,0.)) ;
#15606 = DIRECTION('center_axis',(0.,-1.,0.)) ;
#15607 = DIRECTION('ref_axis',(1.,0.,0.)) ;
#15608 = DIRECTION('',(0.,1.,0.)) ;
#15609 = DIRECTION('center_axis',(0.,-1.,0.)) ;
#15610 = DIRECTION('ref_axis',(1.,0.,0.)) ;
#15611 = DIRECTION('center_axis',(0.,-1.,0.)) ;
#15612 = DIRECTION('ref_axis',(-1.,0.,0.)) ;
#15613 = DIRECTION('center_axis',(0.,1.,0.)) ;
#15614 = DIRECTION('ref_axis',(1.,0.,0.)) ;
#15615 = DIRECTION('center_axis',(0.,1.,0.)) ;
#15616 = DIRECTION('ref_axis',(1.,0.,0.)) ;
#15617 = DIRECTION('',(0.,1.,0.)) ;
#15618 = DIRECTION('center_axis',(0.,1.,0.)) ;
#15619 = DIRECTION('ref_axis',(1.,0.,0.)) ;
#15620 = DIRECTION('center_axis',(0.,1.,0.)) ;
#15621 = DIRECTION('ref_axis',(1.,0.,0.)) ;
#15622 = DIRECTION('center_axis',(0.,1.,0.)) ;
#15623 = DIRECTION('ref_axis',(1.,0.,0.)) ;
#15624 = DIRECTION('center_axis',(0.,1.,0.)) ;
#15625 = DIRECTION('ref_axis',(1.,0.,0.)) ;
#15626 = DIRECTION('',(0.,-1.,0.)) ;
#15627 = DIRECTION('center_axis',(0.,1.,0.)) ;
#15628 = DIRECTION('ref_axis',(1.,0.,0.)) ;
#15629 = DIRECTION('center_axis',(0.,1.,0.)) ;
#15630 = DIRECTION('ref_axis',(1.,0.,0.)) ;
#15631 = DIRECTION('',(0.,-1.,0.)) ;
#15632 = DIRECTION('center_axis',(0.,-1.,0.)) ;
#15633 = DIRECTION('ref_axis',(1.,0.,0.)) ;
#15634 = DIRECTION('center_axis',(0.,-1.,0.)) ;
#15635 = DIRECTION('ref_axis',(-1.,0.,0.)) ;
#15636 = DIRECTION('center_axis',(0.,1.,0.)) ;
#15637 = DIRECTION('ref_axis',(1.,0.,0.)) ;
#15638 = DIRECTION('axis',(0.,0.,1.)) ;
#15639 = DIRECTION('refdir',(1.,0.,0.)) ;
#15640 = DIRECTION('center_axis',(0.,1.,0.)) ;
#15641 = DIRECTION('ref_axis',(1.,0.,0.)) ;
#15642 = DIRECTION('center_axis',(0.,1.,0.)) ;
#15643 = DIRECTION('ref_axis',(1.,0.,0.)) ;
#15644 = DIRECTION('',(0.,1.,0.)) ;
#15645 = DIRECTION('center_axis',(0.,-1.,0.)) ;
#15646 = DIRECTION('ref_axis',(1.,0.,0.)) ;
#15647 = DIRECTION('center_axis',(0.,1.,0.)) ;
#15648 = DIRECTION('ref_axis',(1.,0.,0.)) ;
#15649 = DIRECTION('center_axis',(0.,1.,0.)) ;
#15650 = DIRECTION('ref_axis',(1.,0.,0.)) ;
#15651 = DIRECTION('',(0.,1.,0.)) ;
#15652 = DIRECTION('center_axis',(0.,-1.,0.)) ;
#15653 = DIRECTION('ref_axis',(1.,0.,0.)) ;
#15654 = DIRECTION('center_axis',(0.,1.,0.)) ;
#15655 = DIRECTION('ref_axis',(1.,0.,0.)) ;
#15656 = DIRECTION('center_axis',(0.,1.,0.)) ;
#15657 = DIRECTION('ref_axis',(1.,0.,0.)) ;
#15658 = DIRECTION('',(0.,1.,0.)) ;
#15659 = DIRECTION('center_axis',(0.,-1.,0.)) ;
#15660 = DIRECTION('ref_axis',(1.,0.,0.)) ;
#15661 = DIRECTION('center_axis',(0.,1.,0.)) ;
#15662 = DIRECTION('ref_axis',(1.,0.,0.)) ;
#15663 = DIRECTION('center_axis',(0.,1.,0.)) ;
#15664 = DIRECTION('ref_axis',(1.,0.,0.)) ;
#15665 = DIRECTION('',(0.,1.,0.)) ;
#15666 = DIRECTION('center_axis',(0.,-1.,0.)) ;
#15667 = DIRECTION('ref_axis',(1.,0.,0.)) ;
#15668 = DIRECTION('center_axis',(0.,1.,0.)) ;
#15669 = DIRECTION('ref_axis',(1.,0.,0.)) ;
#15670 = DIRECTION('center_axis',(0.,1.,0.)) ;
#15671 = DIRECTION('ref_axis',(1.,0.,0.)) ;
#15672 = DIRECTION('',(0.,1.,0.)) ;
#15673 = DIRECTION('center_axis',(0.,-1.,0.)) ;
#15674 = DIRECTION('ref_axis',(1.,0.,0.)) ;
#15675 = DIRECTION('center_axis',(0.,1.,0.)) ;
#15676 = DIRECTION('ref_axis',(1.,0.,0.)) ;
#15677 = DIRECTION('center_axis',(0.,1.,0.)) ;
#15678 = DIRECTION('ref_axis',(1.,0.,0.)) ;
#15679 = DIRECTION('',(0.,1.,0.)) ;
#15680 = DIRECTION('center_axis',(0.,-1.,0.)) ;
#15681 = DIRECTION('ref_axis',(1.,0.,0.)) ;
#15682 = DIRECTION('center_axis',(0.,1.,0.)) ;
#15683 = DIRECTION('ref_axis',(1.,0.,0.)) ;
#15684 = DIRECTION('center_axis',(0.,1.,0.)) ;
#15685 = DIRECTION('ref_axis',(1.,0.,0.)) ;
#15686 = DIRECTION('',(0.,1.,0.)) ;
#15687 = DIRECTION('center_axis',(0.,-1.,0.)) ;
#15688 = DIRECTION('ref_axis',(1.,0.,0.)) ;
#15689 = DIRECTION('center_axis',(0.,1.,0.)) ;
#15690 = DIRECTION('ref_axis',(1.,0.,0.)) ;
#15691 = DIRECTION('center_axis',(0.,1.,0.)) ;
#15692 = DIRECTION('ref_axis',(1.,0.,0.)) ;
#15693 = DIRECTION('',(0.,1.,0.)) ;
#15694 = DIRECTION('center_axis',(0.,-1.,0.)) ;
#15695 = DIRECTION('ref_axis',(1.,0.,0.)) ;
#15696 = DIRECTION('center_axis',(0.,1.,0.)) ;
#15697 = DIRECTION('ref_axis',(1.,0.,0.)) ;
#15698 = DIRECTION('center_axis',(0.,1.,0.)) ;
#15699 = DIRECTION('ref_axis',(1.,0.,0.)) ;
#15700 = DIRECTION('',(0.,-1.,0.)) ;
#15701 = DIRECTION('center_axis',(0.,-1.,0.)) ;
#15702 = DIRECTION('ref_axis',(1.,0.,0.)) ;
#15703 = DIRECTION('center_axis',(0.,1.,0.)) ;
#15704 = DIRECTION('ref_axis',(1.,0.,0.)) ;
#15705 = DIRECTION('center_axis',(0.,1.,0.)) ;
#15706 = DIRECTION('ref_axis',(1.,0.,0.)) ;
#15707 = DIRECTION('center_axis',(0.,1.,0.)) ;
#15708 = DIRECTION('ref_axis',(1.,0.,0.)) ;
#15709 = DIRECTION('',(0.,1.,0.)) ;
#15710 = DIRECTION('center_axis',(0.,-1.,0.)) ;
#15711 = DIRECTION('ref_axis',(1.,0.,0.)) ;
#15712 = DIRECTION('center_axis',(0.,1.,0.)) ;
#15713 = DIRECTION('ref_axis',(1.,0.,0.)) ;
#15714 = DIRECTION('center_axis',(0.,1.,0.)) ;
#15715 = DIRECTION('ref_axis',(1.,0.,0.)) ;
#15716 = DIRECTION('',(0.,-1.,0.)) ;
#15717 = DIRECTION('center_axis',(0.,-1.,0.)) ;
#15718 = DIRECTION('ref_axis',(1.,0.,0.)) ;
#15719 = DIRECTION('center_axis',(0.,1.,0.)) ;
#15720 = DIRECTION('ref_axis',(1.,0.,0.)) ;
#15721 = DIRECTION('center_axis',(0.,1.,0.)) ;
#15722 = DIRECTION('ref_axis',(1.,0.,0.)) ;
#15723 = DIRECTION('center_axis',(0.,-1.,0.)) ;
#15724 = DIRECTION('ref_axis',(1.,0.,0.)) ;
#15725 = DIRECTION('',(0.,1.,0.)) ;
#15726 = DIRECTION('center_axis',(0.,-1.,0.)) ;
#15727 = DIRECTION('ref_axis',(1.,0.,0.)) ;
#15728 = DIRECTION('center_axis',(0.,-1.,0.)) ;
#15729 = DIRECTION('ref_axis',(-1.,0.,0.)) ;
#15730 = DIRECTION('center_axis',(0.,1.,0.)) ;
#15731 = DIRECTION('ref_axis',(1.,0.,0.)) ;
#15732 = DIRECTION('center_axis',(0.,1.,0.)) ;
#15733 = DIRECTION('ref_axis',(1.,0.,0.)) ;
#15734 = DIRECTION('center_axis',(0.,1.,0.)) ;
#15735 = DIRECTION('ref_axis',(1.,0.,0.)) ;
#15736 = DIRECTION('',(0.,1.,0.)) ;
#15737 = DIRECTION('center_axis',(0.,1.,0.)) ;
#15738 = DIRECTION('ref_axis',(1.,0.,0.)) ;
#15739 = DIRECTION('center_axis',(0.,1.,0.)) ;
#15740 = DIRECTION('ref_axis',(1.,0.,0.)) ;
#15741 = DIRECTION('',(0.,1.,0.)) ;
#15742 = DIRECTION('center_axis',(0.,1.,0.)) ;
#15743 = DIRECTION('ref_axis',(1.,0.,0.)) ;
#15744 = DIRECTION('center_axis',(0.,1.,0.)) ;
#15745 = DIRECTION('ref_axis',(1.,0.,0.)) ;
#15746 = DIRECTION('center_axis',(0.,1.,0.)) ;
#15747 = DIRECTION('ref_axis',(1.,0.,0.)) ;
#15748 = DIRECTION('center_axis',(0.,1.,0.)) ;
#15749 = DIRECTION('ref_axis',(1.,0.,0.)) ;
#15750 = DIRECTION('',(0.,-1.,0.)) ;
#15751 = DIRECTION('center_axis',(0.,-1.,0.)) ;
#15752 = DIRECTION('ref_axis',(1.,0.,0.)) ;
#15753 = DIRECTION('center_axis',(0.,-1.,0.)) ;
#15754 = DIRECTION('ref_axis',(-1.,0.,0.)) ;
#15755 = DIRECTION('center_axis',(0.,1.,0.)) ;
#15756 = DIRECTION('ref_axis',(1.,0.,0.)) ;
#15757 = DIRECTION('axis',(0.,0.,1.)) ;
#15758 = DIRECTION('refdir',(1.,0.,0.)) ;
#15759 = DIRECTION('center_axis',(0.,1.,0.)) ;
#15760 = DIRECTION('ref_axis',(1.,0.,0.)) ;
#15761 = DIRECTION('center_axis',(0.,1.,0.)) ;
#15762 = DIRECTION('ref_axis',(1.,0.,0.)) ;
#15763 = DIRECTION('',(0.,-1.,0.)) ;
#15764 = DIRECTION('center_axis',(0.,-1.,0.)) ;
#15765 = DIRECTION('ref_axis',(1.,0.,0.)) ;
#15766 = DIRECTION('center_axis',(0.,-1.,0.)) ;
#15767 = DIRECTION('ref_axis',(-1.,0.,0.)) ;
#15768 = DIRECTION('center_axis',(0.,1.,0.)) ;
#15769 = DIRECTION('ref_axis',(1.,0.,0.)) ;
#15770 = DIRECTION('axis',(0.,0.,1.)) ;
#15771 = DIRECTION('refdir',(1.,0.,0.)) ;
#15772 = DIRECTION('center_axis',(0.,1.,0.)) ;
#15773 = DIRECTION('ref_axis',(1.,0.,0.)) ;
#15774 = DIRECTION('center_axis',(0.,1.,0.)) ;
#15775 = DIRECTION('ref_axis',(1.,0.,0.)) ;
#15776 = DIRECTION('',(0.,1.,0.)) ;
#15777 = DIRECTION('center_axis',(0.,-1.,0.)) ;
#15778 = DIRECTION('ref_axis',(1.,0.,0.)) ;
#15779 = DIRECTION('center_axis',(0.,1.,0.)) ;
#15780 = DIRECTION('ref_axis',(1.,0.,0.)) ;
#15781 = DIRECTION('center_axis',(0.,1.,0.)) ;
#15782 = DIRECTION('ref_axis',(1.,0.,0.)) ;
#15783 = DIRECTION('',(0.,1.,0.)) ;
#15784 = DIRECTION('center_axis',(0.,-1.,0.)) ;
#15785 = DIRECTION('ref_axis',(1.,0.,0.)) ;
#15786 = DIRECTION('center_axis',(0.,1.,0.)) ;
#15787 = DIRECTION('ref_axis',(1.,0.,0.)) ;
#15788 = DIRECTION('center_axis',(0.,1.,0.)) ;
#15789 = DIRECTION('ref_axis',(1.,0.,0.)) ;
#15790 = DIRECTION('',(0.,1.,0.)) ;
#15791 = DIRECTION('center_axis',(0.,-1.,0.)) ;
#15792 = DIRECTION('ref_axis',(1.,0.,0.)) ;
#15793 = DIRECTION('center_axis',(0.,1.,0.)) ;
#15794 = DIRECTION('ref_axis',(1.,0.,0.)) ;
#15795 = DIRECTION('center_axis',(0.,1.,0.)) ;
#15796 = DIRECTION('ref_axis',(1.,0.,0.)) ;
#15797 = DIRECTION('',(0.,1.,0.)) ;
#15798 = DIRECTION('center_axis',(0.,-1.,0.)) ;
#15799 = DIRECTION('ref_axis',(1.,0.,0.)) ;
#15800 = DIRECTION('center_axis',(0.,1.,0.)) ;
#15801 = DIRECTION('ref_axis',(1.,0.,0.)) ;
#15802 = DIRECTION('center_axis',(0.,1.,0.)) ;
#15803 = DIRECTION('ref_axis',(1.,0.,0.)) ;
#15804 = DIRECTION('',(0.,1.,0.)) ;
#15805 = DIRECTION('center_axis',(0.,-1.,0.)) ;
#15806 = DIRECTION('ref_axis',(1.,0.,0.)) ;
#15807 = DIRECTION('center_axis',(0.,1.,0.)) ;
#15808 = DIRECTION('ref_axis',(1.,0.,0.)) ;
#15809 = DIRECTION('center_axis',(0.,1.,0.)) ;
#15810 = DIRECTION('ref_axis',(1.,0.,0.)) ;
#15811 = DIRECTION('',(0.,1.,0.)) ;
#15812 = DIRECTION('center_axis',(0.,-1.,0.)) ;
#15813 = DIRECTION('ref_axis',(1.,0.,0.)) ;
#15814 = DIRECTION('center_axis',(0.,1.,0.)) ;
#15815 = DIRECTION('ref_axis',(1.,0.,0.)) ;
#15816 = DIRECTION('center_axis',(0.,1.,0.)) ;
#15817 = DIRECTION('ref_axis',(1.,0.,0.)) ;
#15818 = DIRECTION('',(0.,1.,0.)) ;
#15819 = DIRECTION('center_axis',(0.,-1.,0.)) ;
#15820 = DIRECTION('ref_axis',(1.,0.,0.)) ;
#15821 = DIRECTION('center_axis',(0.,1.,0.)) ;
#15822 = DIRECTION('ref_axis',(1.,0.,0.)) ;
#15823 = DIRECTION('center_axis',(0.,1.,0.)) ;
#15824 = DIRECTION('ref_axis',(1.,0.,0.)) ;
#15825 = DIRECTION('',(0.,-1.,0.)) ;
#15826 = DIRECTION('center_axis',(0.,-1.,0.)) ;
#15827 = DIRECTION('ref_axis',(1.,0.,0.)) ;
#15828 = DIRECTION('center_axis',(0.,-1.,0.)) ;
#15829 = DIRECTION('ref_axis',(-1.,0.,0.)) ;
#15830 = DIRECTION('center_axis',(0.,1.,0.)) ;
#15831 = DIRECTION('ref_axis',(1.,0.,0.)) ;
#15832 = DIRECTION('axis',(0.,0.,1.)) ;
#15833 = DIRECTION('refdir',(1.,0.,0.)) ;
#15834 = DIRECTION('center_axis',(0.,0.,1.)) ;
#15835 = DIRECTION('ref_axis',(1.,0.,0.)) ;
#15836 = DIRECTION('',(1.,0.,0.)) ;
#15837 = DIRECTION('',(0.,-1.,0.)) ;
#15838 = DIRECTION('',(-1.,0.,0.)) ;
#15839 = DIRECTION('',(0.,1.,0.)) ;
#15840 = DIRECTION('center_axis',(0.,-1.,0.)) ;
#15841 = DIRECTION('ref_axis',(0.,0.,-1.)) ;
#15842 = DIRECTION('center_axis',(0.,1.,0.)) ;
#15843 = DIRECTION('ref_axis',(1.,0.,0.)) ;
#15844 = DIRECTION('',(0.,0.,-1.)) ;
#15845 = DIRECTION('',(1.,0.,0.)) ;
#15846 = DIRECTION('center_axis',(0.,0.,1.)) ;
#15847 = DIRECTION('ref_axis',(1.,0.,0.)) ;
#15848 = DIRECTION('',(-1.,0.,0.)) ;
#15849 = DIRECTION('',(0.,-1.,0.)) ;
#15850 = DIRECTION('',(0.,1.,0.)) ;
#15851 = DIRECTION('center_axis',(1.,0.,0.)) ;
#15852 = DIRECTION('ref_axis',(0.,0.,-1.)) ;
#15853 = DIRECTION('',(0.,0.,1.)) ;
#15854 = DIRECTION('center_axis',(0.,1.,0.)) ;
#15855 = DIRECTION('ref_axis',(1.,0.,0.)) ;
#15856 = DIRECTION('center_axis',(0.,-1.,0.)) ;
#15857 = DIRECTION('ref_axis',(1.,0.,0.)) ;
#15858 = DIRECTION('',(0.,-1.,0.)) ;
#15859 = DIRECTION('center_axis',(0.,-1.,0.)) ;
#15860 = DIRECTION('ref_axis',(1.,0.,0.)) ;
#15861 = DIRECTION('center_axis',(0.,-1.,0.)) ;
#15862 = DIRECTION('ref_axis',(1.,0.,0.)) ;
#15863 = DIRECTION('center_axis',(0.,1.,0.)) ;
#15864 = DIRECTION('ref_axis',(1.,0.,0.)) ;
#15865 = DIRECTION('center_axis',(0.,-1.,0.)) ;
#15866 = DIRECTION('ref_axis',(1.,0.,0.)) ;
#15867 = DIRECTION('',(0.,-1.,0.)) ;
#15868 = DIRECTION('center_axis',(0.,1.,0.)) ;
#15869 = DIRECTION('ref_axis',(1.,0.,0.)) ;
#15870 = DIRECTION('center_axis',(0.,-1.,0.)) ;
#15871 = DIRECTION('ref_axis',(-1.,0.,0.)) ;
#15872 = DIRECTION('center_axis',(0.,1.,0.)) ;
#15873 = DIRECTION('ref_axis',(1.,0.,0.)) ;
#15874 = DIRECTION('center_axis',(0.,1.,0.)) ;
#15875 = DIRECTION('ref_axis',(1.,0.,0.)) ;
#15876 = DIRECTION('center_axis',(0.,1.,0.)) ;
#15877 = DIRECTION('ref_axis',(1.,0.,0.)) ;
#15878 = DIRECTION('center_axis',(0.,-1.,0.)) ;
#15879 = DIRECTION('ref_axis',(1.,0.,0.)) ;
#15880 = DIRECTION('',(0.,-1.,0.)) ;
#15881 = DIRECTION('center_axis',(0.,1.,0.)) ;
#15882 = DIRECTION('ref_axis',(1.,0.,0.)) ;
#15883 = DIRECTION('center_axis',(0.,1.,0.)) ;
#15884 = DIRECTION('ref_axis',(1.,0.,0.)) ;
#15885 = DIRECTION('',(0.,1.,0.)) ;
#15886 = DIRECTION('center_axis',(0.,-1.,0.)) ;
#15887 = DIRECTION('ref_axis',(1.,0.,0.)) ;
#15888 = DIRECTION('center_axis',(0.,1.,0.)) ;
#15889 = DIRECTION('ref_axis',(1.,0.,0.)) ;
#15890 = DIRECTION('center_axis',(0.,1.,0.)) ;
#15891 = DIRECTION('ref_axis',(1.,0.,0.)) ;
#15892 = DIRECTION('',(0.,1.,0.)) ;
#15893 = DIRECTION('center_axis',(0.,-1.,0.)) ;
#15894 = DIRECTION('ref_axis',(1.,0.,0.)) ;
#15895 = DIRECTION('center_axis',(0.,1.,0.)) ;
#15896 = DIRECTION('ref_axis',(1.,0.,0.)) ;
#15897 = DIRECTION('center_axis',(0.,1.,0.)) ;
#15898 = DIRECTION('ref_axis',(1.,0.,0.)) ;
#15899 = DIRECTION('',(0.,1.,0.)) ;
#15900 = DIRECTION('center_axis',(0.,-1.,0.)) ;
#15901 = DIRECTION('ref_axis',(1.,0.,0.)) ;
#15902 = DIRECTION('center_axis',(0.,-1.,0.)) ;
#15903 = DIRECTION('ref_axis',(-1.,0.,0.)) ;
#15904 = DIRECTION('center_axis',(0.,-1.,0.)) ;
#15905 = DIRECTION('ref_axis',(1.,0.,0.)) ;
#15906 = DIRECTION('center_axis',(0.,1.,0.)) ;
#15907 = DIRECTION('ref_axis',(1.,0.,0.)) ;
#15908 = DIRECTION('center_axis',(0.,1.,0.)) ;
#15909 = DIRECTION('ref_axis',(1.,0.,0.)) ;
#15910 = DIRECTION('',(0.,-1.,0.)) ;
#15911 = DIRECTION('center_axis',(0.,1.,0.)) ;
#15912 = DIRECTION('ref_axis',(1.,0.,0.)) ;
#15913 = DIRECTION('center_axis',(0.,1.,0.)) ;
#15914 = DIRECTION('ref_axis',(1.,0.,0.)) ;
#15915 = DIRECTION('',(0.,-1.,0.)) ;
#15916 = DIRECTION('center_axis',(0.,-1.,0.)) ;
#15917 = DIRECTION('ref_axis',(1.,0.,0.)) ;
#15918 = DIRECTION('center_axis',(0.,1.,0.)) ;
#15919 = DIRECTION('ref_axis',(1.,0.,0.)) ;
#15920 = DIRECTION('center_axis',(0.,-1.,0.)) ;
#15921 = DIRECTION('ref_axis',(-1.,0.,0.)) ;
#15922 = DIRECTION('center_axis',(0.,1.,0.)) ;
#15923 = DIRECTION('ref_axis',(1.,0.,0.)) ;
#15924 = DIRECTION('axis',(0.,0.,1.)) ;
#15925 = DIRECTION('refdir',(1.,0.,0.)) ;
#15926 = DIRECTION('center_axis',(0.,1.,0.)) ;
#15927 = DIRECTION('ref_axis',(1.,0.,0.)) ;
#15928 = DIRECTION('center_axis',(0.,1.,0.)) ;
#15929 = DIRECTION('ref_axis',(1.,0.,0.)) ;
#15930 = DIRECTION('',(0.,1.,0.)) ;
#15931 = DIRECTION('center_axis',(0.,1.,0.)) ;
#15932 = DIRECTION('ref_axis',(1.,0.,0.)) ;
#15933 = DIRECTION('center_axis',(0.,1.,0.)) ;
#15934 = DIRECTION('ref_axis',(1.,0.,0.)) ;
#15935 = DIRECTION('center_axis',(0.,1.,0.)) ;
#15936 = DIRECTION('ref_axis',(1.,0.,0.)) ;
#15937 = DIRECTION('center_axis',(0.,1.,0.)) ;
#15938 = DIRECTION('ref_axis',(1.,0.,0.)) ;
#15939 = DIRECTION('',(0.,1.,0.)) ;
#15940 = DIRECTION('center_axis',(0.,1.,0.)) ;
#15941 = DIRECTION('ref_axis',(1.,0.,0.)) ;
#15942 = DIRECTION('center_axis',(0.,1.,0.)) ;
#15943 = DIRECTION('ref_axis',(1.,0.,0.)) ;
#15944 = DIRECTION('center_axis',(0.,1.,0.)) ;
#15945 = DIRECTION('ref_axis',(1.,0.,0.)) ;
#15946 = DIRECTION('center_axis',(0.,1.,0.)) ;
#15947 = DIRECTION('ref_axis',(1.,0.,0.)) ;
#15948 = DIRECTION('',(0.,1.,0.)) ;
#15949 = DIRECTION('center_axis',(0.,1.,0.)) ;
#15950 = DIRECTION('ref_axis',(1.,0.,0.)) ;
#15951 = DIRECTION('center_axis',(0.,1.,0.)) ;
#15952 = DIRECTION('ref_axis',(1.,0.,0.)) ;
#15953 = DIRECTION('center_axis',(0.,1.,0.)) ;
#15954 = DIRECTION('ref_axis',(1.,0.,0.)) ;
#15955 = DIRECTION('center_axis',(0.,1.,0.)) ;
#15956 = DIRECTION('ref_axis',(1.,0.,0.)) ;
#15957 = DIRECTION('',(0.,1.,0.)) ;
#15958 = DIRECTION('center_axis',(0.,1.,0.)) ;
#15959 = DIRECTION('ref_axis',(1.,0.,0.)) ;
#15960 = DIRECTION('center_axis',(0.,1.,0.)) ;
#15961 = DIRECTION('ref_axis',(1.,0.,0.)) ;
#15962 = DIRECTION('center_axis',(0.,1.,0.)) ;
#15963 = DIRECTION('ref_axis',(1.,0.,0.)) ;
#15964 = DIRECTION('center_axis',(0.,1.,0.)) ;
#15965 = DIRECTION('ref_axis',(1.,0.,0.)) ;
#15966 = DIRECTION('',(0.,1.,0.)) ;
#15967 = DIRECTION('center_axis',(0.,1.,0.)) ;
#15968 = DIRECTION('ref_axis',(1.,0.,0.)) ;
#15969 = DIRECTION('center_axis',(0.,1.,0.)) ;
#15970 = DIRECTION('ref_axis',(1.,0.,0.)) ;
#15971 = DIRECTION('center_axis',(0.,1.,0.)) ;
#15972 = DIRECTION('ref_axis',(1.,0.,0.)) ;
#15973 = DIRECTION('center_axis',(0.,1.,0.)) ;
#15974 = DIRECTION('ref_axis',(1.,0.,0.)) ;
#15975 = DIRECTION('',(0.,1.,0.)) ;
#15976 = DIRECTION('center_axis',(0.,1.,0.)) ;
#15977 = DIRECTION('ref_axis',(1.,0.,0.)) ;
#15978 = DIRECTION('center_axis',(0.,1.,0.)) ;
#15979 = DIRECTION('ref_axis',(1.,0.,0.)) ;
#15980 = DIRECTION('center_axis',(0.,1.,0.)) ;
#15981 = DIRECTION('ref_axis',(1.,0.,0.)) ;
#15982 = DIRECTION('center_axis',(0.,1.,0.)) ;
#15983 = DIRECTION('ref_axis',(1.,0.,0.)) ;
#15984 = DIRECTION('',(0.,1.,0.)) ;
#15985 = DIRECTION('center_axis',(0.,1.,0.)) ;
#15986 = DIRECTION('ref_axis',(1.,0.,0.)) ;
#15987 = DIRECTION('center_axis',(0.,1.,0.)) ;
#15988 = DIRECTION('ref_axis',(1.,0.,0.)) ;
#15989 = DIRECTION('center_axis',(0.,1.,0.)) ;
#15990 = DIRECTION('ref_axis',(1.,0.,0.)) ;
#15991 = DIRECTION('center_axis',(0.,1.,0.)) ;
#15992 = DIRECTION('ref_axis',(1.,0.,0.)) ;
#15993 = DIRECTION('',(0.,1.,0.)) ;
#15994 = DIRECTION('center_axis',(0.,1.,0.)) ;
#15995 = DIRECTION('ref_axis',(1.,0.,0.)) ;
#15996 = DIRECTION('center_axis',(0.,1.,0.)) ;
#15997 = DIRECTION('ref_axis',(1.,0.,0.)) ;
#15998 = DIRECTION('center_axis',(0.,1.,0.)) ;
#15999 = DIRECTION('ref_axis',(1.,0.,0.)) ;
#16000 = DIRECTION('center_axis',(0.,1.,0.)) ;
#16001 = DIRECTION('ref_axis',(1.,0.,0.)) ;
#16002 = DIRECTION('',(0.,1.,0.)) ;
#16003 = DIRECTION('center_axis',(0.,1.,0.)) ;
#16004 = DIRECTION('ref_axis',(1.,0.,0.)) ;
#16005 = DIRECTION('center_axis',(0.,1.,0.)) ;
#16006 = DIRECTION('ref_axis',(1.,0.,0.)) ;
#16007 = DIRECTION('center_axis',(0.,1.,0.)) ;
#16008 = DIRECTION('ref_axis',(1.,0.,0.)) ;
#16009 = DIRECTION('center_axis',(0.,1.,0.)) ;
#16010 = DIRECTION('ref_axis',(1.,0.,0.)) ;
#16011 = DIRECTION('',(0.,1.,0.)) ;
#16012 = DIRECTION('center_axis',(0.,1.,0.)) ;
#16013 = DIRECTION('ref_axis',(1.,0.,0.)) ;
#16014 = DIRECTION('center_axis',(0.,1.,0.)) ;
#16015 = DIRECTION('ref_axis',(1.,0.,0.)) ;
#16016 = DIRECTION('center_axis',(0.,1.,0.)) ;
#16017 = DIRECTION('ref_axis',(1.,0.,0.)) ;
#16018 = DIRECTION('center_axis',(0.,1.,0.)) ;
#16019 = DIRECTION('ref_axis',(1.,0.,0.)) ;
#16020 = DIRECTION('',(0.,1.,0.)) ;
#16021 = DIRECTION('center_axis',(0.,1.,0.)) ;
#16022 = DIRECTION('ref_axis',(1.,0.,0.)) ;
#16023 = DIRECTION('center_axis',(0.,1.,0.)) ;
#16024 = DIRECTION('ref_axis',(1.,0.,0.)) ;
#16025 = DIRECTION('center_axis',(0.,1.,0.)) ;
#16026 = DIRECTION('ref_axis',(1.,0.,0.)) ;
#16027 = DIRECTION('center_axis',(0.,1.,0.)) ;
#16028 = DIRECTION('ref_axis',(1.,0.,0.)) ;
#16029 = DIRECTION('',(0.,1.,0.)) ;
#16030 = DIRECTION('center_axis',(0.,1.,0.)) ;
#16031 = DIRECTION('ref_axis',(1.,0.,0.)) ;
#16032 = DIRECTION('center_axis',(0.,1.,0.)) ;
#16033 = DIRECTION('ref_axis',(1.,0.,0.)) ;
#16034 = DIRECTION('center_axis',(0.,1.,0.)) ;
#16035 = DIRECTION('ref_axis',(1.,0.,0.)) ;
#16036 = DIRECTION('center_axis',(0.,1.,0.)) ;
#16037 = DIRECTION('ref_axis',(1.,0.,0.)) ;
#16038 = DIRECTION('',(0.,1.,0.)) ;
#16039 = DIRECTION('center_axis',(0.,1.,0.)) ;
#16040 = DIRECTION('ref_axis',(1.,0.,0.)) ;
#16041 = DIRECTION('center_axis',(0.,1.,0.)) ;
#16042 = DIRECTION('ref_axis',(1.,0.,0.)) ;
#16043 = DIRECTION('center_axis',(0.,1.,0.)) ;
#16044 = DIRECTION('ref_axis',(1.,0.,0.)) ;
#16045 = DIRECTION('center_axis',(0.,1.,0.)) ;
#16046 = DIRECTION('ref_axis',(1.,0.,0.)) ;
#16047 = DIRECTION('',(0.,1.,0.)) ;
#16048 = DIRECTION('center_axis',(0.,1.,0.)) ;
#16049 = DIRECTION('ref_axis',(1.,0.,0.)) ;
#16050 = DIRECTION('center_axis',(0.,1.,0.)) ;
#16051 = DIRECTION('ref_axis',(1.,0.,0.)) ;
#16052 = DIRECTION('center_axis',(0.,1.,0.)) ;
#16053 = DIRECTION('ref_axis',(1.,0.,0.)) ;
#16054 = DIRECTION('center_axis',(0.,1.,0.)) ;
#16055 = DIRECTION('ref_axis',(1.,0.,0.)) ;
#16056 = DIRECTION('',(0.,1.,0.)) ;
#16057 = DIRECTION('center_axis',(0.,1.,0.)) ;
#16058 = DIRECTION('ref_axis',(1.,0.,0.)) ;
#16059 = DIRECTION('center_axis',(0.,1.,0.)) ;
#16060 = DIRECTION('ref_axis',(1.,0.,0.)) ;
#16061 = DIRECTION('center_axis',(0.,1.,0.)) ;
#16062 = DIRECTION('ref_axis',(1.,0.,0.)) ;
#16063 = DIRECTION('center_axis',(0.,1.,0.)) ;
#16064 = DIRECTION('ref_axis',(1.,0.,0.)) ;
#16065 = DIRECTION('',(0.,1.,0.)) ;
#16066 = DIRECTION('center_axis',(0.,1.,0.)) ;
#16067 = DIRECTION('ref_axis',(1.,0.,0.)) ;
#16068 = DIRECTION('center_axis',(0.,1.,0.)) ;
#16069 = DIRECTION('ref_axis',(1.,0.,0.)) ;
#16070 = DIRECTION('center_axis',(0.,1.,0.)) ;
#16071 = DIRECTION('ref_axis',(1.,0.,0.)) ;
#16072 = DIRECTION('center_axis',(0.,1.,0.)) ;
#16073 = DIRECTION('ref_axis',(1.,0.,0.)) ;
#16074 = DIRECTION('',(0.,1.,0.)) ;
#16075 = DIRECTION('center_axis',(0.,1.,0.)) ;
#16076 = DIRECTION('ref_axis',(1.,0.,0.)) ;
#16077 = DIRECTION('center_axis',(0.,1.,0.)) ;
#16078 = DIRECTION('ref_axis',(1.,0.,0.)) ;
#16079 = DIRECTION('center_axis',(0.,1.,0.)) ;
#16080 = DIRECTION('ref_axis',(1.,0.,0.)) ;
#16081 = DIRECTION('center_axis',(0.,1.,0.)) ;
#16082 = DIRECTION('ref_axis',(1.,0.,0.)) ;
#16083 = DIRECTION('',(0.,1.,0.)) ;
#16084 = DIRECTION('center_axis',(0.,1.,0.)) ;
#16085 = DIRECTION('ref_axis',(1.,0.,0.)) ;
#16086 = DIRECTION('center_axis',(0.,1.,0.)) ;
#16087 = DIRECTION('ref_axis',(1.,0.,0.)) ;
#16088 = DIRECTION('center_axis',(0.,1.,0.)) ;
#16089 = DIRECTION('ref_axis',(1.,0.,0.)) ;
#16090 = DIRECTION('center_axis',(0.,1.,0.)) ;
#16091 = DIRECTION('ref_axis',(1.,0.,0.)) ;
#16092 = DIRECTION('',(0.,1.,0.)) ;
#16093 = DIRECTION('center_axis',(0.,1.,0.)) ;
#16094 = DIRECTION('ref_axis',(1.,0.,0.)) ;
#16095 = DIRECTION('center_axis',(0.,1.,0.)) ;
#16096 = DIRECTION('ref_axis',(1.,0.,0.)) ;
#16097 = DIRECTION('center_axis',(0.,1.,0.)) ;
#16098 = DIRECTION('ref_axis',(1.,0.,0.)) ;
#16099 = DIRECTION('center_axis',(0.,1.,0.)) ;
#16100 = DIRECTION('ref_axis',(1.,0.,0.)) ;
#16101 = DIRECTION('',(0.,1.,0.)) ;
#16102 = DIRECTION('center_axis',(0.,1.,0.)) ;
#16103 = DIRECTION('ref_axis',(1.,0.,0.)) ;
#16104 = DIRECTION('center_axis',(0.,1.,0.)) ;
#16105 = DIRECTION('ref_axis',(1.,0.,0.)) ;
#16106 = DIRECTION('center_axis',(0.,1.,0.)) ;
#16107 = DIRECTION('ref_axis',(1.,0.,0.)) ;
#16108 = DIRECTION('center_axis',(0.,1.,0.)) ;
#16109 = DIRECTION('ref_axis',(1.,0.,0.)) ;
#16110 = DIRECTION('',(0.,1.,0.)) ;
#16111 = DIRECTION('center_axis',(0.,1.,0.)) ;
#16112 = DIRECTION('ref_axis',(1.,0.,0.)) ;
#16113 = DIRECTION('center_axis',(0.,1.,0.)) ;
#16114 = DIRECTION('ref_axis',(1.,0.,0.)) ;
#16115 = DIRECTION('center_axis',(0.,1.,0.)) ;
#16116 = DIRECTION('ref_axis',(1.,0.,0.)) ;
#16117 = DIRECTION('center_axis',(0.,1.,0.)) ;
#16118 = DIRECTION('ref_axis',(1.,0.,0.)) ;
#16119 = DIRECTION('',(0.,1.,0.)) ;
#16120 = DIRECTION('center_axis',(0.,1.,0.)) ;
#16121 = DIRECTION('ref_axis',(1.,0.,0.)) ;
#16122 = DIRECTION('center_axis',(0.,1.,0.)) ;
#16123 = DIRECTION('ref_axis',(1.,0.,0.)) ;
#16124 = DIRECTION('center_axis',(0.,1.,0.)) ;
#16125 = DIRECTION('ref_axis',(1.,0.,0.)) ;
#16126 = DIRECTION('center_axis',(0.,1.,0.)) ;
#16127 = DIRECTION('ref_axis',(1.,0.,0.)) ;
#16128 = DIRECTION('',(0.,1.,0.)) ;
#16129 = DIRECTION('center_axis',(0.,1.,0.)) ;
#16130 = DIRECTION('ref_axis',(1.,0.,0.)) ;
#16131 = DIRECTION('center_axis',(0.,1.,0.)) ;
#16132 = DIRECTION('ref_axis',(1.,0.,0.)) ;
#16133 = DIRECTION('center_axis',(0.,1.,0.)) ;
#16134 = DIRECTION('ref_axis',(1.,0.,0.)) ;
#16135 = DIRECTION('center_axis',(0.,1.,0.)) ;
#16136 = DIRECTION('ref_axis',(1.,0.,0.)) ;
#16137 = DIRECTION('',(0.,1.,0.)) ;
#16138 = DIRECTION('center_axis',(0.,1.,0.)) ;
#16139 = DIRECTION('ref_axis',(1.,0.,0.)) ;
#16140 = DIRECTION('center_axis',(0.,1.,0.)) ;
#16141 = DIRECTION('ref_axis',(1.,0.,0.)) ;
#16142 = DIRECTION('center_axis',(0.,1.,0.)) ;
#16143 = DIRECTION('ref_axis',(1.,0.,0.)) ;
#16144 = DIRECTION('center_axis',(0.,1.,0.)) ;
#16145 = DIRECTION('ref_axis',(1.,0.,0.)) ;
#16146 = DIRECTION('',(0.,1.,0.)) ;
#16147 = DIRECTION('center_axis',(0.,-1.,0.)) ;
#16148 = DIRECTION('ref_axis',(1.,0.,0.)) ;
#16149 = DIRECTION('center_axis',(0.,1.,0.)) ;
#16150 = DIRECTION('ref_axis',(1.,0.,0.)) ;
#16151 = DIRECTION('center_axis',(0.,1.,0.)) ;
#16152 = DIRECTION('ref_axis',(1.,0.,0.)) ;
#16153 = DIRECTION('',(0.,1.,0.)) ;
#16154 = DIRECTION('center_axis',(0.,-1.,0.)) ;
#16155 = DIRECTION('ref_axis',(1.,0.,0.)) ;
#16156 = DIRECTION('center_axis',(0.,1.,0.)) ;
#16157 = DIRECTION('ref_axis',(1.,0.,0.)) ;
#16158 = DIRECTION('center_axis',(0.,1.,0.)) ;
#16159 = DIRECTION('ref_axis',(1.,0.,0.)) ;
#16160 = DIRECTION('',(0.,1.,0.)) ;
#16161 = DIRECTION('center_axis',(0.,-1.,0.)) ;
#16162 = DIRECTION('ref_axis',(1.,0.,0.)) ;
#16163 = DIRECTION('center_axis',(0.,1.,0.)) ;
#16164 = DIRECTION('ref_axis',(1.,0.,0.)) ;
#16165 = DIRECTION('center_axis',(0.,1.,0.)) ;
#16166 = DIRECTION('ref_axis',(1.,0.,0.)) ;
#16167 = DIRECTION('',(0.,1.,0.)) ;
#16168 = DIRECTION('center_axis',(0.,-1.,0.)) ;
#16169 = DIRECTION('ref_axis',(1.,0.,0.)) ;
#16170 = DIRECTION('center_axis',(0.,1.,0.)) ;
#16171 = DIRECTION('ref_axis',(1.,0.,0.)) ;
#16172 = DIRECTION('center_axis',(0.,1.,0.)) ;
#16173 = DIRECTION('ref_axis',(1.,0.,0.)) ;
#16174 = DIRECTION('',(0.,1.,0.)) ;
#16175 = DIRECTION('center_axis',(0.,-1.,0.)) ;
#16176 = DIRECTION('ref_axis',(1.,0.,0.)) ;
#16177 = DIRECTION('center_axis',(0.,1.,0.)) ;
#16178 = DIRECTION('ref_axis',(1.,0.,0.)) ;
#16179 = DIRECTION('center_axis',(0.,1.,0.)) ;
#16180 = DIRECTION('ref_axis',(1.,0.,0.)) ;
#16181 = DIRECTION('',(0.,1.,0.)) ;
#16182 = DIRECTION('center_axis',(0.,-1.,0.)) ;
#16183 = DIRECTION('ref_axis',(1.,0.,0.)) ;
#16184 = DIRECTION('center_axis',(0.,1.,0.)) ;
#16185 = DIRECTION('ref_axis',(1.,0.,0.)) ;
#16186 = DIRECTION('center_axis',(0.,1.,0.)) ;
#16187 = DIRECTION('ref_axis',(1.,0.,0.)) ;
#16188 = DIRECTION('',(0.,1.,0.)) ;
#16189 = DIRECTION('center_axis',(0.,-1.,0.)) ;
#16190 = DIRECTION('ref_axis',(1.,0.,0.)) ;
#16191 = DIRECTION('center_axis',(0.,1.,0.)) ;
#16192 = DIRECTION('ref_axis',(1.,0.,0.)) ;
#16193 = DIRECTION('center_axis',(0.,1.,0.)) ;
#16194 = DIRECTION('ref_axis',(1.,0.,0.)) ;
#16195 = DIRECTION('',(0.,1.,0.)) ;
#16196 = DIRECTION('center_axis',(0.,-1.,0.)) ;
#16197 = DIRECTION('ref_axis',(1.,0.,0.)) ;
#16198 = DIRECTION('center_axis',(0.,1.,0.)) ;
#16199 = DIRECTION('ref_axis',(1.,0.,0.)) ;
#16200 = DIRECTION('center_axis',(0.,1.,0.)) ;
#16201 = DIRECTION('ref_axis',(1.,0.,0.)) ;
#16202 = DIRECTION('',(0.,1.,0.)) ;
#16203 = DIRECTION('center_axis',(0.,-1.,0.)) ;
#16204 = DIRECTION('ref_axis',(1.,0.,0.)) ;
#16205 = DIRECTION('center_axis',(0.,1.,0.)) ;
#16206 = DIRECTION('ref_axis',(1.,0.,0.)) ;
#16207 = DIRECTION('center_axis',(0.,1.,0.)) ;
#16208 = DIRECTION('ref_axis',(1.,0.,0.)) ;
#16209 = DIRECTION('',(0.,1.,0.)) ;
#16210 = DIRECTION('center_axis',(0.,-1.,0.)) ;
#16211 = DIRECTION('ref_axis',(1.,0.,0.)) ;
#16212 = DIRECTION('center_axis',(0.,1.,0.)) ;
#16213 = DIRECTION('ref_axis',(1.,0.,0.)) ;
#16214 = DIRECTION('center_axis',(0.,1.,0.)) ;
#16215 = DIRECTION('ref_axis',(1.,0.,0.)) ;
#16216 = DIRECTION('',(0.,1.,0.)) ;
#16217 = DIRECTION('center_axis',(0.,-1.,0.)) ;
#16218 = DIRECTION('ref_axis',(1.,0.,0.)) ;
#16219 = DIRECTION('center_axis',(0.,1.,0.)) ;
#16220 = DIRECTION('ref_axis',(1.,0.,0.)) ;
#16221 = DIRECTION('center_axis',(0.,1.,0.)) ;
#16222 = DIRECTION('ref_axis',(1.,0.,0.)) ;
#16223 = DIRECTION('',(0.,1.,0.)) ;
#16224 = DIRECTION('center_axis',(0.,-1.,0.)) ;
#16225 = DIRECTION('ref_axis',(1.,0.,0.)) ;
#16226 = DIRECTION('center_axis',(0.,1.,0.)) ;
#16227 = DIRECTION('ref_axis',(1.,0.,0.)) ;
#16228 = DIRECTION('center_axis',(0.,1.,0.)) ;
#16229 = DIRECTION('ref_axis',(1.,0.,0.)) ;
#16230 = DIRECTION('',(0.,1.,0.)) ;
#16231 = DIRECTION('center_axis',(0.,-1.,0.)) ;
#16232 = DIRECTION('ref_axis',(1.,0.,0.)) ;
#16233 = DIRECTION('center_axis',(0.,1.,0.)) ;
#16234 = DIRECTION('ref_axis',(1.,0.,0.)) ;
#16235 = DIRECTION('center_axis',(0.,1.,0.)) ;
#16236 = DIRECTION('ref_axis',(1.,0.,0.)) ;
#16237 = DIRECTION('',(0.,1.,0.)) ;
#16238 = DIRECTION('center_axis',(0.,-1.,0.)) ;
#16239 = DIRECTION('ref_axis',(1.,0.,0.)) ;
#16240 = DIRECTION('center_axis',(0.,1.,0.)) ;
#16241 = DIRECTION('ref_axis',(1.,0.,0.)) ;
#16242 = DIRECTION('center_axis',(0.,1.,0.)) ;
#16243 = DIRECTION('ref_axis',(1.,0.,0.)) ;
#16244 = DIRECTION('',(0.,1.,0.)) ;
#16245 = DIRECTION('center_axis',(0.,-1.,0.)) ;
#16246 = DIRECTION('ref_axis',(1.,0.,0.)) ;
#16247 = DIRECTION('center_axis',(0.,1.,0.)) ;
#16248 = DIRECTION('ref_axis',(1.,0.,0.)) ;
#16249 = DIRECTION('center_axis',(0.,1.,0.)) ;
#16250 = DIRECTION('ref_axis',(1.,0.,0.)) ;
#16251 = DIRECTION('',(0.,1.,0.)) ;
#16252 = DIRECTION('center_axis',(0.,-1.,0.)) ;
#16253 = DIRECTION('ref_axis',(1.,0.,0.)) ;
#16254 = DIRECTION('center_axis',(0.,1.,0.)) ;
#16255 = DIRECTION('ref_axis',(1.,0.,0.)) ;
#16256 = DIRECTION('center_axis',(0.,1.,0.)) ;
#16257 = DIRECTION('ref_axis',(1.,0.,0.)) ;
#16258 = DIRECTION('',(0.,1.,0.)) ;
#16259 = DIRECTION('center_axis',(0.,-1.,0.)) ;
#16260 = DIRECTION('ref_axis',(1.,0.,0.)) ;
#16261 = DIRECTION('center_axis',(0.,1.,0.)) ;
#16262 = DIRECTION('ref_axis',(1.,0.,0.)) ;
#16263 = DIRECTION('center_axis',(0.,1.,0.)) ;
#16264 = DIRECTION('ref_axis',(1.,0.,0.)) ;
#16265 = DIRECTION('',(0.,1.,0.)) ;
#16266 = DIRECTION('center_axis',(0.,-1.,0.)) ;
#16267 = DIRECTION('ref_axis',(1.,0.,0.)) ;
#16268 = DIRECTION('center_axis',(0.,1.,0.)) ;
#16269 = DIRECTION('ref_axis',(1.,0.,0.)) ;
#16270 = DIRECTION('center_axis',(0.,1.,0.)) ;
#16271 = DIRECTION('ref_axis',(1.,0.,0.)) ;
#16272 = DIRECTION('',(0.,1.,0.)) ;
#16273 = DIRECTION('center_axis',(0.,-1.,0.)) ;
#16274 = DIRECTION('ref_axis',(1.,0.,0.)) ;
#16275 = DIRECTION('center_axis',(0.,1.,0.)) ;
#16276 = DIRECTION('ref_axis',(1.,0.,0.)) ;
#16277 = DIRECTION('center_axis',(0.,1.,0.)) ;
#16278 = DIRECTION('ref_axis',(1.,0.,0.)) ;
#16279 = DIRECTION('',(0.,1.,0.)) ;
#16280 = DIRECTION('center_axis',(0.,-1.,0.)) ;
#16281 = DIRECTION('ref_axis',(1.,0.,0.)) ;
#16282 = DIRECTION('center_axis',(0.,1.,0.)) ;
#16283 = DIRECTION('ref_axis',(1.,0.,0.)) ;
#16284 = DIRECTION('center_axis',(0.,1.,0.)) ;
#16285 = DIRECTION('ref_axis',(1.,0.,0.)) ;
#16286 = DIRECTION('',(0.,1.,0.)) ;
#16287 = DIRECTION('center_axis',(0.,-1.,0.)) ;
#16288 = DIRECTION('ref_axis',(1.,0.,0.)) ;
#16289 = DIRECTION('center_axis',(0.,1.,0.)) ;
#16290 = DIRECTION('ref_axis',(1.,0.,0.)) ;
#16291 = DIRECTION('center_axis',(0.,1.,0.)) ;
#16292 = DIRECTION('ref_axis',(1.,0.,0.)) ;
#16293 = DIRECTION('',(0.,1.,0.)) ;
#16294 = DIRECTION('center_axis',(0.,-1.,0.)) ;
#16295 = DIRECTION('ref_axis',(1.,0.,0.)) ;
#16296 = DIRECTION('center_axis',(0.,1.,0.)) ;
#16297 = DIRECTION('ref_axis',(1.,0.,0.)) ;
#16298 = DIRECTION('center_axis',(0.,1.,0.)) ;
#16299 = DIRECTION('ref_axis',(1.,0.,0.)) ;
#16300 = DIRECTION('',(0.,1.,0.)) ;
#16301 = DIRECTION('center_axis',(0.,-1.,0.)) ;
#16302 = DIRECTION('ref_axis',(1.,0.,0.)) ;
#16303 = DIRECTION('center_axis',(0.,1.,0.)) ;
#16304 = DIRECTION('ref_axis',(1.,0.,0.)) ;
#16305 = DIRECTION('center_axis',(0.,1.,0.)) ;
#16306 = DIRECTION('ref_axis',(1.,0.,0.)) ;
#16307 = DIRECTION('',(0.,1.,0.)) ;
#16308 = DIRECTION('center_axis',(0.,-1.,0.)) ;
#16309 = DIRECTION('ref_axis',(1.,0.,0.)) ;
#16310 = DIRECTION('center_axis',(0.,1.,0.)) ;
#16311 = DIRECTION('ref_axis',(1.,0.,0.)) ;
#16312 = DIRECTION('center_axis',(0.,1.,0.)) ;
#16313 = DIRECTION('ref_axis',(1.,0.,0.)) ;
#16314 = DIRECTION('',(0.,1.,0.)) ;
#16315 = DIRECTION('center_axis',(0.,-1.,0.)) ;
#16316 = DIRECTION('ref_axis',(1.,0.,0.)) ;
#16317 = DIRECTION('center_axis',(0.,1.,0.)) ;
#16318 = DIRECTION('ref_axis',(1.,0.,0.)) ;
#16319 = DIRECTION('center_axis',(0.,1.,0.)) ;
#16320 = DIRECTION('ref_axis',(1.,0.,0.)) ;
#16321 = DIRECTION('',(0.,1.,0.)) ;
#16322 = DIRECTION('center_axis',(0.,-1.,0.)) ;
#16323 = DIRECTION('ref_axis',(1.,0.,0.)) ;
#16324 = DIRECTION('center_axis',(0.,1.,0.)) ;
#16325 = DIRECTION('ref_axis',(1.,0.,0.)) ;
#16326 = DIRECTION('center_axis',(0.,1.,0.)) ;
#16327 = DIRECTION('ref_axis',(1.,0.,0.)) ;
#16328 = DIRECTION('',(0.,1.,0.)) ;
#16329 = DIRECTION('center_axis',(0.,-1.,0.)) ;
#16330 = DIRECTION('ref_axis',(1.,0.,0.)) ;
#16331 = DIRECTION('center_axis',(0.,1.,0.)) ;
#16332 = DIRECTION('ref_axis',(1.,0.,0.)) ;
#16333 = DIRECTION('center_axis',(0.,1.,0.)) ;
#16334 = DIRECTION('ref_axis',(1.,0.,0.)) ;
#16335 = DIRECTION('',(0.,1.,0.)) ;
#16336 = DIRECTION('center_axis',(0.,-1.,0.)) ;
#16337 = DIRECTION('ref_axis',(1.,0.,0.)) ;
#16338 = DIRECTION('center_axis',(0.,1.,0.)) ;
#16339 = DIRECTION('ref_axis',(1.,0.,0.)) ;
#16340 = DIRECTION('center_axis',(0.,1.,0.)) ;
#16341 = DIRECTION('ref_axis',(1.,0.,0.)) ;
#16342 = DIRECTION('',(0.,-1.,0.)) ;
#16343 = DIRECTION('center_axis',(0.,-1.,0.)) ;
#16344 = DIRECTION('ref_axis',(1.,0.,0.)) ;
#16345 = DIRECTION('center_axis',(0.,-1.,0.)) ;
#16346 = DIRECTION('ref_axis',(-1.,0.,0.)) ;
#16347 = DIRECTION('center_axis',(0.,1.,0.)) ;
#16348 = DIRECTION('ref_axis',(1.,0.,0.)) ;
#16349 = DIRECTION('axis',(0.,0.,1.)) ;
#16350 = DIRECTION('refdir',(1.,0.,0.)) ;
#16351 = DIRECTION('center_axis',(0.,-1.,0.)) ;
#16352 = DIRECTION('ref_axis',(-1.,0.,0.)) ;
#16353 = DIRECTION('center_axis',(0.,1.,0.)) ;
#16354 = DIRECTION('ref_axis',(1.,0.,0.)) ;
#16355 = DIRECTION('center_axis',(0.,-1.,0.)) ;
#16356 = DIRECTION('ref_axis',(1.,0.,0.)) ;
#16357 = DIRECTION('center_axis',(0.,1.,0.)) ;
#16358 = DIRECTION('ref_axis',(1.,0.,0.)) ;
#16359 = DIRECTION('center_axis',(0.,-1.,0.)) ;
#16360 = DIRECTION('ref_axis',(1.,0.,0.)) ;
#16361 = DIRECTION('center_axis',(0.,1.,0.)) ;
#16362 = DIRECTION('ref_axis',(1.,0.,0.)) ;
#16363 = DIRECTION('center_axis',(0.,1.,0.)) ;
#16364 = DIRECTION('ref_axis',(1.,0.,0.)) ;
#16365 = DIRECTION('',(0.,-1.,0.)) ;
#16366 = DIRECTION('center_axis',(0.,1.,0.)) ;
#16367 = DIRECTION('ref_axis',(1.,0.,0.)) ;
#16368 = DIRECTION('',(0.,1.,0.)) ;
#16369 = DIRECTION('center_axis',(0.,-1.,0.)) ;
#16370 = DIRECTION('ref_axis',(-1.,0.,0.)) ;
#16371 = DIRECTION('center_axis',(0.,-1.,0.)) ;
#16372 = DIRECTION('ref_axis',(1.,0.,0.)) ;
#16373 = DIRECTION('center_axis',(0.,1.,0.)) ;
#16374 = DIRECTION('ref_axis',(1.,0.,0.)) ;
#16375 = DIRECTION('center_axis',(0.,1.,0.)) ;
#16376 = DIRECTION('ref_axis',(1.,0.,0.)) ;
#16377 = DIRECTION('center_axis',(0.,1.,0.)) ;
#16378 = DIRECTION('ref_axis',(1.,0.,0.)) ;
#16379 = DIRECTION('',(0.,-1.,0.)) ;
#16380 = DIRECTION('center_axis',(0.,1.,0.)) ;
#16381 = DIRECTION('ref_axis',(1.,0.,0.)) ;
#16382 = DIRECTION('center_axis',(0.,-1.,0.)) ;
#16383 = DIRECTION('ref_axis',(1.,0.,0.)) ;
#16384 = DIRECTION('center_axis',(0.,1.,0.)) ;
#16385 = DIRECTION('ref_axis',(1.,0.,0.)) ;
#16386 = DIRECTION('',(0.,1.,0.)) ;
#16387 = DIRECTION('axis',(0.,0.,1.)) ;
#16388 = DIRECTION('refdir',(1.,0.,0.)) ;
#16389 = DIRECTION('center_axis',(0.,-1.,0.)) ;
#16390 = DIRECTION('ref_axis',(-1.,0.,0.)) ;
#16391 = DIRECTION('center_axis',(0.,1.,0.)) ;
#16392 = DIRECTION('ref_axis',(1.,0.,0.)) ;
#16393 = DIRECTION('center_axis',(0.,-1.,0.)) ;
#16394 = DIRECTION('ref_axis',(1.,0.,0.)) ;
#16395 = DIRECTION('center_axis',(0.,1.,0.)) ;
#16396 = DIRECTION('ref_axis',(1.,0.,0.)) ;
#16397 = DIRECTION('center_axis',(0.,-1.,0.)) ;
#16398 = DIRECTION('ref_axis',(1.,0.,0.)) ;
#16399 = DIRECTION('center_axis',(0.,1.,0.)) ;
#16400 = DIRECTION('ref_axis',(1.,0.,0.)) ;
#16401 = DIRECTION('center_axis',(0.,1.,0.)) ;
#16402 = DIRECTION('ref_axis',(1.,0.,0.)) ;
#16403 = DIRECTION('',(0.,-1.,0.)) ;
#16404 = DIRECTION('center_axis',(0.,1.,0.)) ;
#16405 = DIRECTION('ref_axis',(1.,0.,0.)) ;
#16406 = DIRECTION('',(0.,1.,0.)) ;
#16407 = DIRECTION('center_axis',(0.,-1.,0.)) ;
#16408 = DIRECTION('ref_axis',(-1.,0.,0.)) ;
#16409 = DIRECTION('center_axis',(0.,-1.,0.)) ;
#16410 = DIRECTION('ref_axis',(1.,0.,0.)) ;
#16411 = DIRECTION('center_axis',(0.,1.,0.)) ;
#16412 = DIRECTION('ref_axis',(1.,0.,0.)) ;
#16413 = DIRECTION('center_axis',(0.,1.,0.)) ;
#16414 = DIRECTION('ref_axis',(1.,0.,0.)) ;
#16415 = DIRECTION('center_axis',(0.,1.,0.)) ;
#16416 = DIRECTION('ref_axis',(1.,0.,0.)) ;
#16417 = DIRECTION('',(0.,-1.,0.)) ;
#16418 = DIRECTION('center_axis',(0.,1.,0.)) ;
#16419 = DIRECTION('ref_axis',(1.,0.,0.)) ;
#16420 = DIRECTION('center_axis',(0.,-1.,0.)) ;
#16421 = DIRECTION('ref_axis',(1.,0.,0.)) ;
#16422 = DIRECTION('center_axis',(0.,1.,0.)) ;
#16423 = DIRECTION('ref_axis',(1.,0.,0.)) ;
#16424 = DIRECTION('',(0.,1.,0.)) ;
#16425 = DIRECTION('axis',(0.,0.,1.)) ;
#16426 = DIRECTION('refdir',(1.,0.,0.)) ;
#16427 = DIRECTION('center_axis',(0.,1.,0.)) ;
#16428 = DIRECTION('ref_axis',(1.,0.,0.)) ;
#16429 = DIRECTION('center_axis',(0.,1.,0.)) ;
#16430 = DIRECTION('ref_axis',(1.,0.,0.)) ;
#16431 = DIRECTION('',(0.,1.,0.)) ;
#16432 = DIRECTION('center_axis',(0.,-1.,0.)) ;
#16433 = DIRECTION('ref_axis',(1.,0.,0.)) ;
#16434 = DIRECTION('center_axis',(0.,1.,0.)) ;
#16435 = DIRECTION('ref_axis',(1.,0.,0.)) ;
#16436 = DIRECTION('center_axis',(0.,1.,0.)) ;
#16437 = DIRECTION('ref_axis',(1.,0.,0.)) ;
#16438 = DIRECTION('',(0.,-1.,0.)) ;
#16439 = DIRECTION('center_axis',(0.,-1.,0.)) ;
#16440 = DIRECTION('ref_axis',(1.,0.,0.)) ;
#16441 = DIRECTION('center_axis',(0.,-1.,0.)) ;
#16442 = DIRECTION('ref_axis',(-1.,0.,0.)) ;
#16443 = DIRECTION('center_axis',(0.,1.,0.)) ;
#16444 = DIRECTION('ref_axis',(1.,0.,0.)) ;
#16445 = DIRECTION('axis',(0.,0.,1.)) ;
#16446 = DIRECTION('refdir',(1.,0.,0.)) ;
#16447 = DIRECTION('center_axis',(1.,0.,0.)) ;
#16448 = DIRECTION('ref_axis',(0.,0.,-1.)) ;
#16449 = DIRECTION('',(0.,-1.,0.)) ;
#16450 = DIRECTION('',(0.,0.,-1.)) ;
#16451 = DIRECTION('',(0.,1.,0.)) ;
#16452 = DIRECTION('',(0.,0.,1.)) ;
#16453 = DIRECTION('center_axis',(-1.,0.,0.)) ;
#16454 = DIRECTION('ref_axis',(0.,0.,1.)) ;
#16455 = DIRECTION('',(0.,1.,0.)) ;
#16456 = DIRECTION('',(0.,0.,-1.)) ;
#16457 = DIRECTION('',(0.,-1.,0.)) ;
#16458 = DIRECTION('',(0.,0.,1.)) ;
#16459 = DIRECTION('center_axis',(0.,1.,0.)) ;
#16460 = DIRECTION('ref_axis',(1.,0.,0.)) ;
#16461 = DIRECTION('center_axis',(0.,1.,0.)) ;
#16462 = DIRECTION('ref_axis',(1.,0.,0.)) ;
#16463 = DIRECTION('center_axis',(0.,-1.,0.)) ;
#16464 = DIRECTION('ref_axis',(1.,0.,0.)) ;
#16465 = DIRECTION('center_axis',(0.,1.,0.)) ;
#16466 = DIRECTION('ref_axis',(-1.83697019872103E-16,0.,1.)) ;
#16467 = DIRECTION('center_axis',(0.,1.,0.)) ;
#16468 = DIRECTION('ref_axis',(1.,0.,0.)) ;
#16469 = DIRECTION('center_axis',(0.,1.,0.)) ;
#16470 = DIRECTION('ref_axis',(-1.83697019872103E-16,0.,1.)) ;
#16471 = DIRECTION('center_axis',(0.,-1.,0.)) ;
#16472 = DIRECTION('ref_axis',(1.,0.,0.)) ;
#16473 = DIRECTION('center_axis',(0.,-1.,0.)) ;
#16474 = DIRECTION('ref_axis',(-1.,0.,0.)) ;
#16475 = DIRECTION('axis',(0.,0.,1.)) ;
#16476 = DIRECTION('refdir',(1.,0.,0.)) ;
#16477 = DIRECTION('center_axis',(0.,0.,1.)) ;
#16478 = DIRECTION('ref_axis',(1.,0.,0.)) ;
#16479 = DIRECTION('',(-1.,0.,0.)) ;
#16480 = DIRECTION('',(0.,1.,0.)) ;
#16481 = DIRECTION('',(1.,0.,0.)) ;
#16482 = DIRECTION('',(0.,-1.,0.)) ;
#16483 = DIRECTION('center_axis',(0.,0.,1.)) ;
#16484 = DIRECTION('ref_axis',(1.,0.,0.)) ;
#16485 = DIRECTION('',(1.,0.,0.)) ;
#16486 = DIRECTION('',(0.,1.,0.)) ;
#16487 = DIRECTION('',(-1.,0.,0.)) ;
#16488 = DIRECTION('',(0.,-1.,0.)) ;
#16489 = DIRECTION('center_axis',(-1.,0.,0.)) ;
#16490 = DIRECTION('ref_axis',(0.,0.,1.)) ;
#16491 = DIRECTION('',(0.,0.,1.)) ;
#16492 = DIRECTION('',(0.,0.,-1.)) ;
#16493 = DIRECTION('center_axis',(0.,-1.,0.)) ;
#16494 = DIRECTION('ref_axis',(-1.,0.,0.)) ;
#16495 = DIRECTION('center_axis',(0.,-1.,0.)) ;
#16496 = DIRECTION('ref_axis',(1.,0.,0.)) ;
#16497 = DIRECTION('center_axis',(0.,1.,0.)) ;
#16498 = DIRECTION('ref_axis',(1.,0.,0.)) ;
#16499 = DIRECTION('center_axis',(0.,1.,0.)) ;
#16500 = DIRECTION('ref_axis',(-1.,0.,1.22464679914735E-16)) ;
#16501 = DIRECTION('center_axis',(0.,-1.,0.)) ;
#16502 = DIRECTION('ref_axis',(1.,0.,0.)) ;
#16503 = DIRECTION('center_axis',(0.5,0.,0.866025403784438)) ;
#16504 = DIRECTION('ref_axis',(0.866025403784438,0.,-0.5)) ;
#16505 = DIRECTION('',(0.,-1.,0.)) ;
#16506 = DIRECTION('',(0.866025403784438,0.,-0.5)) ;
#16507 = DIRECTION('',(0.,-1.,0.)) ;
#16508 = DIRECTION('',(-0.866025403784438,0.,0.5)) ;
#16509 = DIRECTION('center_axis',(0.5,0.,0.866025403784438)) ;
#16510 = DIRECTION('ref_axis',(0.866025403784438,0.,-0.5)) ;
#16511 = DIRECTION('',(0.,1.,0.)) ;
#16512 = DIRECTION('',(0.866025403784438,0.,-0.5)) ;
#16513 = DIRECTION('',(0.,1.,0.)) ;
#16514 = DIRECTION('',(-0.866025403784438,0.,0.5)) ;
#16515 = DIRECTION('center_axis',(-0.866025403784438,0.,0.5)) ;
#16516 = DIRECTION('ref_axis',(0.5,0.,0.866025403784438)) ;
#16517 = DIRECTION('',(-0.5,0.,-0.866025403784438)) ;
#16518 = DIRECTION('',(-0.5,0.,-0.866025403784438)) ;
#16519 = DIRECTION('center_axis',(0.,1.,0.)) ;
#16520 = DIRECTION('ref_axis',(1.,0.,0.)) ;
#16521 = DIRECTION('center_axis',(0.,-1.,0.)) ;
#16522 = DIRECTION('ref_axis',(1.,0.,0.)) ;
#16523 = DIRECTION('',(0.,1.,0.)) ;
#16524 = DIRECTION('center_axis',(0.,1.,0.)) ;
#16525 = DIRECTION('ref_axis',(1.,0.,0.)) ;
#16526 = DIRECTION('center_axis',(0.,1.,0.)) ;
#16527 = DIRECTION('ref_axis',(1.,0.,0.)) ;
#16528 = DIRECTION('center_axis',(0.,1.,0.)) ;
#16529 = DIRECTION('ref_axis',(1.,0.,0.)) ;
#16530 = DIRECTION('',(0.,-1.,0.)) ;
#16531 = DIRECTION('center_axis',(0.,-1.,0.)) ;
#16532 = DIRECTION('ref_axis',(1.,0.,0.)) ;
#16533 = DIRECTION('center_axis',(0.,1.,0.)) ;
#16534 = DIRECTION('ref_axis',(1.,0.,0.)) ;
#16535 = DIRECTION('',(-0.5,0.,0.866025403784439)) ;
#16536 = DIRECTION('',(-0.866025403784439,0.,-0.5)) ;
#16537 = DIRECTION('',(0.5,0.,-0.866025403784439)) ;
#16538 = DIRECTION('center_axis',(0.,1.,0.)) ;
#16539 = DIRECTION('ref_axis',(1.,0.,0.)) ;
#16540 = DIRECTION('',(1.83697019872103E-16,0.,1.)) ;
#16541 = DIRECTION('',(-1.,0.,1.83697019872103E-16)) ;
#16542 = DIRECTION('',(-1.83697019872103E-16,0.,-1.)) ;
#16543 = DIRECTION('center_axis',(0.,1.,0.)) ;
#16544 = DIRECTION('ref_axis',(1.,0.,0.)) ;
#16545 = DIRECTION('',(0.5,0.,0.866025403784438)) ;
#16546 = DIRECTION('',(-0.866025403784438,0.,0.5)) ;
#16547 = DIRECTION('',(-0.5,0.,-0.866025403784438)) ;
#16548 = DIRECTION('center_axis',(0.,1.,0.)) ;
#16549 = DIRECTION('ref_axis',(1.,0.,0.)) ;
#16550 = DIRECTION('',(0.866025403784439,0.,0.5)) ;
#16551 = DIRECTION('',(-0.5,0.,0.866025403784439)) ;
#16552 = DIRECTION('',(-0.866025403784439,0.,-0.5)) ;
#16553 = DIRECTION('center_axis',(0.,1.,0.)) ;
#16554 = DIRECTION('ref_axis',(1.,0.,0.)) ;
#16555 = DIRECTION('',(1.,0.,-1.22464679914735E-16)) ;
#16556 = DIRECTION('',(1.22464679914735E-16,0.,1.)) ;
#16557 = DIRECTION('',(-1.,0.,1.22464679914735E-16)) ;
#16558 = DIRECTION('center_axis',(0.,1.,0.)) ;
#16559 = DIRECTION('ref_axis',(1.,0.,0.)) ;
#16560 = DIRECTION('',(0.866025403784439,0.,-0.5)) ;
#16561 = DIRECTION('',(0.5,0.,0.866025403784439)) ;
#16562 = DIRECTION('',(-0.866025403784439,0.,0.5)) ;
#16563 = DIRECTION('center_axis',(0.,1.,0.)) ;
#16564 = DIRECTION('ref_axis',(1.,0.,0.)) ;
#16565 = DIRECTION('',(0.5,0.,-0.866025403784439)) ;
#16566 = DIRECTION('',(0.866025403784439,0.,0.5)) ;
#16567 = DIRECTION('',(-0.5,0.,0.866025403784439)) ;
#16568 = DIRECTION('center_axis',(0.,1.,0.)) ;
#16569 = DIRECTION('ref_axis',(1.,0.,0.)) ;
#16570 = DIRECTION('',(-6.12323399573677E-17,0.,-1.)) ;
#16571 = DIRECTION('',(1.,0.,-6.12323399573677E-17)) ;
#16572 = DIRECTION('',(6.12323399573677E-17,0.,1.)) ;
#16573 = DIRECTION('center_axis',(0.,1.,0.)) ;
#16574 = DIRECTION('ref_axis',(1.,0.,0.)) ;
#16575 = DIRECTION('',(-0.5,0.,-0.866025403784439)) ;
#16576 = DIRECTION('',(0.866025403784439,0.,-0.5)) ;
#16577 = DIRECTION('',(0.5,0.,0.866025403784439)) ;
#16578 = DIRECTION('center_axis',(0.,1.,0.)) ;
#16579 = DIRECTION('ref_axis',(1.,0.,0.)) ;
#16580 = DIRECTION('',(-0.866025403784439,0.,-0.5)) ;
#16581 = DIRECTION('',(0.5,0.,-0.866025403784439)) ;
#16582 = DIRECTION('',(0.866025403784439,0.,0.5)) ;
#16583 = DIRECTION('center_axis',(0.,1.,0.)) ;
#16584 = DIRECTION('ref_axis',(1.,0.,0.)) ;
#16585 = DIRECTION('',(-1.,0.,0.)) ;
#16586 = DIRECTION('',(0.,0.,-1.)) ;
#16587 = DIRECTION('',(1.,0.,0.)) ;
#16588 = DIRECTION('center_axis',(0.866025403784439,0.,0.5)) ;
#16589 = DIRECTION('ref_axis',(0.5,0.,-0.866025403784439)) ;
#16590 = DIRECTION('',(0.5,0.,-0.866025403784439)) ;
#16591 = DIRECTION('',(0.,1.,0.)) ;
#16592 = DIRECTION('center_axis',(0.866025403784439,0.,0.5)) ;
#16593 = DIRECTION('ref_axis',(0.5,0.,-0.866025403784439)) ;
#16594 = DIRECTION('',(0.,-1.,0.)) ;
#16595 = DIRECTION('',(0.,-1.,0.)) ;
#16596 = DIRECTION('',(-0.5,0.,0.866025403784439)) ;
#16597 = DIRECTION('center_axis',(-0.5,0.,0.866025403784439)) ;
#16598 = DIRECTION('ref_axis',(0.866025403784439,0.,0.5)) ;
#16599 = DIRECTION('',(-0.866025403784439,0.,-0.5)) ;
#16600 = DIRECTION('center_axis',(0.,1.,0.)) ;
#16601 = DIRECTION('ref_axis',(1.,0.,0.)) ;
#16602 = DIRECTION('center_axis',(0.,-1.,0.)) ;
#16603 = DIRECTION('ref_axis',(1.,0.,0.)) ;
#16604 = DIRECTION('',(0.,1.,0.)) ;
#16605 = DIRECTION('center_axis',(1.,0.,-1.83697019872103E-16)) ;
#16606 = DIRECTION('ref_axis',(-1.83697019872103E-16,0.,-1.)) ;
#16607 = DIRECTION('',(0.,-1.,0.)) ;
#16608 = DIRECTION('',(0.,-1.,0.)) ;
#16609 = DIRECTION('',(1.83697019872103E-16,0.,1.)) ;
#16610 = DIRECTION('center_axis',(1.,0.,-1.83697019872103E-16)) ;
#16611 = DIRECTION('ref_axis',(-1.83697019872103E-16,0.,-1.)) ;
#16612 = DIRECTION('',(-1.83697019872103E-16,0.,-1.)) ;
#16613 = DIRECTION('',(0.,1.,0.)) ;
#16614 = DIRECTION('center_axis',(1.83697019872103E-16,0.,1.)) ;
#16615 = DIRECTION('ref_axis',(1.,0.,-1.83697019872103E-16)) ;
#16616 = DIRECTION('',(-1.,0.,1.83697019872103E-16)) ;
#16617 = DIRECTION('center_axis',(0.,1.,0.)) ;
#16618 = DIRECTION('ref_axis',(1.,0.,0.)) ;
#16619 = DIRECTION('center_axis',(0.,-1.,0.)) ;
#16620 = DIRECTION('ref_axis',(1.,0.,0.)) ;
#16621 = DIRECTION('',(0.,1.,0.)) ;
#16622 = DIRECTION('center_axis',(0.866025403784438,0.,-0.5)) ;
#16623 = DIRECTION('ref_axis',(-0.5,0.,-0.866025403784438)) ;
#16624 = DIRECTION('',(-0.5,0.,-0.866025403784438)) ;
#16625 = DIRECTION('',(0.,1.,0.)) ;
#16626 = DIRECTION('center_axis',(0.866025403784438,0.,-0.5)) ;
#16627 = DIRECTION('ref_axis',(-0.5,0.,-0.866025403784438)) ;
#16628 = DIRECTION('',(0.,-1.,0.)) ;
#16629 = DIRECTION('',(0.,-1.,0.)) ;
#16630 = DIRECTION('',(0.5,0.,0.866025403784438)) ;
#16631 = DIRECTION('center_axis',(0.5,0.,0.866025403784438)) ;
#16632 = DIRECTION('ref_axis',(0.866025403784438,0.,-0.5)) ;
#16633 = DIRECTION('',(-0.866025403784438,0.,0.5)) ;
#16634 = DIRECTION('center_axis',(0.,1.,0.)) ;
#16635 = DIRECTION('ref_axis',(1.,0.,0.)) ;
#16636 = DIRECTION('center_axis',(0.,-1.,0.)) ;
#16637 = DIRECTION('ref_axis',(1.,0.,0.)) ;
#16638 = DIRECTION('',(0.,1.,0.)) ;
#16639 = DIRECTION('center_axis',(0.5,0.,-0.866025403784439)) ;
#16640 = DIRECTION('ref_axis',(-0.866025403784439,0.,-0.5)) ;
#16641 = DIRECTION('',(0.,-1.,0.)) ;
#16642 = DIRECTION('',(0.,-1.,0.)) ;
#16643 = DIRECTION('',(0.866025403784439,0.,0.5)) ;
#16644 = DIRECTION('center_axis',(0.5,0.,-0.866025403784439)) ;
#16645 = DIRECTION('ref_axis',(-0.866025403784439,0.,-0.5)) ;
#16646 = DIRECTION('',(-0.866025403784439,0.,-0.5)) ;
#16647 = DIRECTION('',(0.,1.,0.)) ;
#16648 = DIRECTION('center_axis',(0.866025403784439,0.,0.5)) ;
#16649 = DIRECTION('ref_axis',(0.5,0.,-0.866025403784439)) ;
#16650 = DIRECTION('',(-0.5,0.,0.866025403784439)) ;
#16651 = DIRECTION('center_axis',(0.,1.,0.)) ;
#16652 = DIRECTION('ref_axis',(1.,0.,0.)) ;
#16653 = DIRECTION('center_axis',(0.,-1.,0.)) ;
#16654 = DIRECTION('ref_axis',(1.,0.,0.)) ;
#16655 = DIRECTION('',(0.,1.,0.)) ;
#16656 = DIRECTION('center_axis',(-1.22464679914735E-16,0.,-1.)) ;
#16657 = DIRECTION('ref_axis',(-1.,0.,1.22464679914735E-16)) ;
#16658 = DIRECTION('',(-1.,0.,1.22464679914735E-16)) ;
#16659 = DIRECTION('',(0.,1.,0.)) ;
#16660 = DIRECTION('center_axis',(-1.22464679914735E-16,0.,-1.)) ;
#16661 = DIRECTION('ref_axis',(-1.,0.,1.22464679914735E-16)) ;
#16662 = DIRECTION('',(0.,-1.,0.)) ;
#16663 = DIRECTION('',(0.,-1.,0.)) ;
#16664 = DIRECTION('',(1.,0.,-1.22464679914735E-16)) ;
#16665 = DIRECTION('center_axis',(1.,0.,-1.22464679914735E-16)) ;
#16666 = DIRECTION('ref_axis',(-1.22464679914735E-16,0.,-1.)) ;
#16667 = DIRECTION('',(1.22464679914735E-16,0.,1.)) ;
#16668 = DIRECTION('center_axis',(0.,1.,0.)) ;
#16669 = DIRECTION('ref_axis',(1.,0.,0.)) ;
#16670 = DIRECTION('center_axis',(0.,-1.,0.)) ;
#16671 = DIRECTION('ref_axis',(1.,0.,0.)) ;
#16672 = DIRECTION('',(0.,1.,0.)) ;
#16673 = DIRECTION('center_axis',(-0.5,0.,-0.866025403784439)) ;
#16674 = DIRECTION('ref_axis',(-0.866025403784439,0.,0.5)) ;
#16675 = DIRECTION('',(0.,-1.,0.)) ;
#16676 = DIRECTION('',(0.,-1.,0.)) ;
#16677 = DIRECTION('',(0.866025403784439,0.,-0.5)) ;
#16678 = DIRECTION('center_axis',(-0.5,0.,-0.866025403784439)) ;
#16679 = DIRECTION('ref_axis',(-0.866025403784439,0.,0.5)) ;
#16680 = DIRECTION('',(-0.866025403784439,0.,0.5)) ;
#16681 = DIRECTION('',(0.,1.,0.)) ;
#16682 = DIRECTION('center_axis',(0.866025403784439,0.,-0.5)) ;
#16683 = DIRECTION('ref_axis',(-0.5,0.,-0.866025403784439)) ;
#16684 = DIRECTION('',(0.5,0.,0.866025403784439)) ;
#16685 = DIRECTION('center_axis',(0.,1.,0.)) ;
#16686 = DIRECTION('ref_axis',(1.,0.,0.)) ;
#16687 = DIRECTION('center_axis',(0.,-1.,0.)) ;
#16688 = DIRECTION('ref_axis',(1.,0.,0.)) ;
#16689 = DIRECTION('',(0.,1.,0.)) ;
#16690 = DIRECTION('center_axis',(-0.866025403784439,0.,-0.5)) ;
#16691 = DIRECTION('ref_axis',(-0.5,0.,0.866025403784439)) ;
#16692 = DIRECTION('',(-0.5,0.,0.866025403784439)) ;
#16693 = DIRECTION('',(0.,1.,0.)) ;
#16694 = DIRECTION('center_axis',(-0.866025403784439,0.,-0.5)) ;
#16695 = DIRECTION('ref_axis',(-0.5,0.,0.866025403784439)) ;
#16696 = DIRECTION('',(0.,-1.,0.)) ;
#16697 = DIRECTION('',(0.,-1.,0.)) ;
#16698 = DIRECTION('',(0.5,0.,-0.866025403784439)) ;
#16699 = DIRECTION('center_axis',(0.5,0.,-0.866025403784439)) ;
#16700 = DIRECTION('ref_axis',(-0.866025403784439,0.,-0.5)) ;
#16701 = DIRECTION('',(0.866025403784439,0.,0.5)) ;
#16702 = DIRECTION('center_axis',(0.,1.,0.)) ;
#16703 = DIRECTION('ref_axis',(1.,0.,0.)) ;
#16704 = DIRECTION('center_axis',(0.,-1.,0.)) ;
#16705 = DIRECTION('ref_axis',(1.,0.,0.)) ;
#16706 = DIRECTION('',(0.,1.,0.)) ;
#16707 = DIRECTION('center_axis',(-1.,0.,6.12323399573677E-17)) ;
#16708 = DIRECTION('ref_axis',(6.12323399573677E-17,0.,1.)) ;
#16709 = DIRECTION('',(0.,-1.,0.)) ;
#16710 = DIRECTION('',(0.,-1.,0.)) ;
#16711 = DIRECTION('',(-6.12323399573677E-17,0.,-1.)) ;
#16712 = DIRECTION('center_axis',(-1.,0.,6.12323399573677E-17)) ;
#16713 = DIRECTION('ref_axis',(6.12323399573677E-17,0.,1.)) ;
#16714 = DIRECTION('',(6.12323399573677E-17,0.,1.)) ;
#16715 = DIRECTION('',(0.,1.,0.)) ;
#16716 = DIRECTION('center_axis',(-6.12323399573677E-17,0.,-1.)) ;
#16717 = DIRECTION('ref_axis',(-1.,0.,6.12323399573677E-17)) ;
#16718 = DIRECTION('',(1.,0.,-6.12323399573677E-17)) ;
#16719 = DIRECTION('center_axis',(0.,1.,0.)) ;
#16720 = DIRECTION('ref_axis',(1.,0.,0.)) ;
#16721 = DIRECTION('center_axis',(0.,-1.,0.)) ;
#16722 = DIRECTION('ref_axis',(1.,0.,0.)) ;
#16723 = DIRECTION('',(0.,1.,0.)) ;
#16724 = DIRECTION('center_axis',(-0.866025403784439,0.,0.5)) ;
#16725 = DIRECTION('ref_axis',(0.5,0.,0.866025403784439)) ;
#16726 = DIRECTION('',(0.5,0.,0.866025403784439)) ;
#16727 = DIRECTION('',(0.,1.,0.)) ;
#16728 = DIRECTION('center_axis',(-0.866025403784439,0.,0.5)) ;
#16729 = DIRECTION('ref_axis',(0.5,0.,0.866025403784439)) ;
#16730 = DIRECTION('',(0.,-1.,0.)) ;
#16731 = DIRECTION('',(0.,-1.,0.)) ;
#16732 = DIRECTION('',(-0.5,0.,-0.866025403784439)) ;
#16733 = DIRECTION('center_axis',(-0.5,0.,-0.866025403784439)) ;
#16734 = DIRECTION('ref_axis',(-0.866025403784439,0.,0.5)) ;
#16735 = DIRECTION('',(0.866025403784439,0.,-0.5)) ;
#16736 = DIRECTION('center_axis',(0.,1.,0.)) ;
#16737 = DIRECTION('ref_axis',(1.,0.,0.)) ;
#16738 = DIRECTION('center_axis',(0.,-1.,0.)) ;
#16739 = DIRECTION('ref_axis',(1.,0.,0.)) ;
#16740 = DIRECTION('',(0.,1.,0.)) ;
#16741 = DIRECTION('center_axis',(-0.5,0.,0.866025403784439)) ;
#16742 = DIRECTION('ref_axis',(0.866025403784439,0.,0.5)) ;
#16743 = DIRECTION('',(0.,-1.,0.)) ;
#16744 = DIRECTION('',(0.,-1.,0.)) ;
#16745 = DIRECTION('',(-0.866025403784439,0.,-0.5)) ;
#16746 = DIRECTION('center_axis',(-0.5,0.,0.866025403784439)) ;
#16747 = DIRECTION('ref_axis',(0.866025403784439,0.,0.5)) ;
#16748 = DIRECTION('',(0.866025403784439,0.,0.5)) ;
#16749 = DIRECTION('',(0.,1.,0.)) ;
#16750 = DIRECTION('center_axis',(-0.866025403784439,0.,-0.5)) ;
#16751 = DIRECTION('ref_axis',(-0.5,0.,0.866025403784439)) ;
#16752 = DIRECTION('',(0.5,0.,-0.866025403784439)) ;
#16753 = DIRECTION('center_axis',(0.,1.,0.)) ;
#16754 = DIRECTION('ref_axis',(1.,0.,0.)) ;
#16755 = DIRECTION('center_axis',(0.,-1.,0.)) ;
#16756 = DIRECTION('ref_axis',(1.,0.,0.)) ;
#16757 = DIRECTION('',(0.,1.,0.)) ;
#16758 = DIRECTION('center_axis',(0.,0.,1.)) ;
#16759 = DIRECTION('ref_axis',(1.,0.,0.)) ;
#16760 = DIRECTION('',(1.,0.,0.)) ;
#16761 = DIRECTION('',(0.,1.,0.)) ;
#16762 = DIRECTION('center_axis',(0.,0.,1.)) ;
#16763 = DIRECTION('ref_axis',(1.,0.,0.)) ;
#16764 = DIRECTION('',(0.,-1.,0.)) ;
#16765 = DIRECTION('',(-1.,0.,0.)) ;
#16766 = DIRECTION('center_axis',(-1.,0.,0.)) ;
#16767 = DIRECTION('ref_axis',(0.,0.,1.)) ;
#16768 = DIRECTION('',(0.,0.,-1.)) ;
#16769 = DIRECTION('center_axis',(0.,1.,0.)) ;
#16770 = DIRECTION('ref_axis',(1.,0.,0.)) ;
#16771 = DIRECTION('center_axis',(0.,1.,0.)) ;
#16772 = DIRECTION('ref_axis',(1.,0.,0.)) ;
#16773 = DIRECTION('',(0.,-1.,0.)) ;
#16774 = DIRECTION('center_axis',(0.,-1.,0.)) ;
#16775 = DIRECTION('ref_axis',(-1.,0.,0.)) ;
#16776 = DIRECTION('axis',(0.,0.,1.)) ;
#16777 = DIRECTION('refdir',(1.,0.,0.)) ;
#16778 = DIRECTION('center_axis',(0.,0.,1.)) ;
#16779 = DIRECTION('ref_axis',(1.,0.,0.)) ;
#16780 = DIRECTION('',(0.,1.,0.)) ;
#16781 = DIRECTION('',(-1.,0.,0.)) ;
#16782 = DIRECTION('',(0.,-1.,0.)) ;
#16783 = DIRECTION('',(1.,0.,0.)) ;
#16784 = DIRECTION('center_axis',(0.,0.,1.)) ;
#16785 = DIRECTION('ref_axis',(1.,0.,0.)) ;
#16786 = DIRECTION('',(0.,-1.,0.)) ;
#16787 = DIRECTION('',(-1.,0.,0.)) ;
#16788 = DIRECTION('',(0.,1.,0.)) ;
#16789 = DIRECTION('',(1.,0.,0.)) ;
#16790 = DIRECTION('center_axis',(0.,1.,0.)) ;
#16791 = DIRECTION('ref_axis',(0.,0.,1.)) ;
#16792 = DIRECTION('',(0.,0.,-1.)) ;
#16793 = DIRECTION('',(0.,0.,-1.)) ;
#16794 = DIRECTION('center_axis',(1.,0.,0.)) ;
#16795 = DIRECTION('ref_axis',(0.,0.,-1.)) ;
#16796 = DIRECTION('',(0.,0.,-1.)) ;
#16797 = DIRECTION('center_axis',(0.,-1.,0.)) ;
#16798 = DIRECTION('ref_axis',(0.,0.,-1.)) ;
#16799 = DIRECTION('',(0.,0.,-1.)) ;
#16800 = DIRECTION('center_axis',(-1.,0.,0.)) ;
#16801 = DIRECTION('ref_axis',(0.,0.,1.)) ;
#16802 = DIRECTION('axis',(0.,0.,1.)) ;
#16803 = DIRECTION('refdir',(1.,0.,0.)) ;
#16804 = DIRECTION('center_axis',(0.,1.,0.)) ;
#16805 = DIRECTION('ref_axis',(1.,0.,0.)) ;
#16806 = DIRECTION('center_axis',(0.,1.,0.)) ;
#16807 = DIRECTION('ref_axis',(1.,0.,0.)) ;
#16808 = DIRECTION('',(0.,1.,0.)) ;
#16809 = DIRECTION('center_axis',(0.,-1.,0.)) ;
#16810 = DIRECTION('ref_axis',(1.,0.,0.)) ;
#16811 = DIRECTION('center_axis',(0.,1.,0.)) ;
#16812 = DIRECTION('ref_axis',(1.,0.,0.)) ;
#16813 = DIRECTION('center_axis',(0.,1.,0.)) ;
#16814 = DIRECTION('ref_axis',(1.,0.,0.)) ;
#16815 = DIRECTION('',(0.,-1.,0.)) ;
#16816 = DIRECTION('center_axis',(0.,-1.,0.)) ;
#16817 = DIRECTION('ref_axis',(1.,0.,0.)) ;
#16818 = DIRECTION('center_axis',(0.,-1.,0.)) ;
#16819 = DIRECTION('ref_axis',(-1.,0.,0.)) ;
#16820 = DIRECTION('center_axis',(0.,1.,0.)) ;
#16821 = DIRECTION('ref_axis',(1.,0.,0.)) ;
#16822 = DIRECTION('axis',(0.,0.,1.)) ;
#16823 = DIRECTION('refdir',(1.,0.,0.)) ;
#16824 = DIRECTION('center_axis',(0.,0.,1.)) ;
#16825 = DIRECTION('ref_axis',(1.,0.,0.)) ;
#16826 = DIRECTION('',(1.,0.,0.)) ;
#16827 = DIRECTION('',(0.,1.,0.)) ;
#16828 = DIRECTION('',(-1.,0.,0.)) ;
#16829 = DIRECTION('',(0.,-1.,0.)) ;
#16830 = DIRECTION('center_axis',(-1.,0.,0.)) ;
#16831 = DIRECTION('ref_axis',(0.,0.,1.)) ;
#16832 = DIRECTION('',(0.,0.,1.)) ;
#16833 = DIRECTION('',(0.,0.,-1.)) ;
#16834 = DIRECTION('',(0.,-1.,0.)) ;
#16835 = DIRECTION('center_axis',(0.,1.,0.)) ;
#16836 = DIRECTION('ref_axis',(0.,0.,1.)) ;
#16837 = DIRECTION('',(-1.,0.,0.)) ;
#16838 = DIRECTION('',(0.,0.,-1.)) ;
#16839 = DIRECTION('center_axis',(1.,0.,0.)) ;
#16840 = DIRECTION('ref_axis',(0.,0.,-1.)) ;
#16841 = DIRECTION('',(0.,0.,-1.)) ;
#16842 = DIRECTION('',(0.,1.,0.)) ;
#16843 = DIRECTION('center_axis',(0.,-1.,0.)) ;
#16844 = DIRECTION('ref_axis',(0.,0.,-1.)) ;
#16845 = DIRECTION('',(-1.,0.,0.)) ;
#16846 = DIRECTION('',(0.,0.,-1.)) ;
#16847 = DIRECTION('',(1.,0.,0.)) ;
#16848 = DIRECTION('',(0.,0.,-1.)) ;
#16849 = DIRECTION('',(-1.,0.,0.)) ;
#16850 = DIRECTION('center_axis',(0.,0.,1.)) ;
#16851 = DIRECTION('ref_axis',(1.,0.,0.)) ;
#16852 = DIRECTION('',(0.,-1.,0.)) ;
#16853 = DIRECTION('',(1.,0.,0.)) ;
#16854 = DIRECTION('',(0.,1.,0.)) ;
#16855 = DIRECTION('center_axis',(0.,0.,1.)) ;
#16856 = DIRECTION('ref_axis',(1.,0.,0.)) ;
#16857 = DIRECTION('',(0.,-1.,0.)) ;
#16858 = DIRECTION('',(-1.,0.,0.)) ;
#16859 = DIRECTION('',(0.,1.,0.)) ;
#16860 = DIRECTION('center_axis',(0.,1.,0.)) ;
#16861 = DIRECTION('ref_axis',(0.,0.,1.)) ;
#16862 = DIRECTION('',(0.,0.,-1.)) ;
#16863 = DIRECTION('',(0.,0.,-1.)) ;
#16864 = DIRECTION('center_axis',(1.,0.,0.)) ;
#16865 = DIRECTION('ref_axis',(0.,0.,-1.)) ;
#16866 = DIRECTION('center_axis',(-1.,0.,0.)) ;
#16867 = DIRECTION('ref_axis',(0.,0.,1.)) ;
#16868 = DIRECTION('axis',(0.,0.,1.)) ;
#16869 = DIRECTION('refdir',(1.,0.,0.)) ;
#16870 = DIRECTION('center_axis',(0.,1.,0.)) ;
#16871 = DIRECTION('ref_axis',(1.,0.,0.)) ;
#16872 = DIRECTION('center_axis',(0.,1.,0.)) ;
#16873 = DIRECTION('ref_axis',(1.,0.,0.)) ;
#16874 = DIRECTION('',(0.,-1.,0.)) ;
#16875 = DIRECTION('center_axis',(0.,-1.,0.)) ;
#16876 = DIRECTION('ref_axis',(1.,0.,0.)) ;
#16877 = DIRECTION('center_axis',(0.,-1.,0.)) ;
#16878 = DIRECTION('ref_axis',(-1.,0.,0.)) ;
#16879 = DIRECTION('center_axis',(0.,1.,0.)) ;
#16880 = DIRECTION('ref_axis',(1.,0.,0.)) ;
#16881 = DIRECTION('center_axis',(0.,1.,0.)) ;
#16882 = DIRECTION('ref_axis',(1.,0.,0.)) ;
#16883 = DIRECTION('',(0.,1.,0.)) ;
#16884 = DIRECTION('center_axis',(0.,-1.,0.)) ;
#16885 = DIRECTION('ref_axis',(1.,0.,0.)) ;
#16886 = DIRECTION('center_axis',(0.,1.,0.)) ;
#16887 = DIRECTION('ref_axis',(-0.997582534658001,0.,0.0694916293183479)) ;
#16888 = DIRECTION('',(0.,1.,0.)) ;
#16889 = DIRECTION('center_axis',(0.,-1.,0.)) ;
#16890 = DIRECTION('ref_axis',(1.,0.,0.)) ;
#16891 = DIRECTION('',(0.,-1.,0.)) ;
#16892 = DIRECTION('center_axis',(0.,1.,0.)) ;
#16893 = DIRECTION('ref_axis',(1.,0.,0.)) ;
#16894 = DIRECTION('center_axis',(0.,1.,0.)) ;
#16895 = DIRECTION('ref_axis',(1.,0.,0.)) ;
#16896 = DIRECTION('',(0.,-1.,0.)) ;
#16897 = DIRECTION('center_axis',(0.,1.,0.)) ;
#16898 = DIRECTION('ref_axis',(1.,0.,0.)) ;
#16899 = DIRECTION('',(0.,1.,0.)) ;
#16900 = DIRECTION('center_axis',(0.,-1.,0.)) ;
#16901 = DIRECTION('ref_axis',(1.,0.,0.)) ;
#16902 = DIRECTION('center_axis',(0.,1.,0.)) ;
#16903 = DIRECTION('ref_axis',(1.,0.,0.)) ;
#16904 = DIRECTION('',(0.,1.,0.)) ;
#16905 = DIRECTION('center_axis',(0.,-1.,0.)) ;
#16906 = DIRECTION('ref_axis',(1.,0.,0.)) ;
#16907 = DIRECTION('',(0.,-1.,0.)) ;
#16908 = DIRECTION('center_axis',(0.,1.,0.)) ;
#16909 = DIRECTION('ref_axis',(1.,0.,0.)) ;
#16910 = DIRECTION('center_axis',(0.997582534658001,0.,-0.0694916293183465)) ;
#16911 = DIRECTION('ref_axis',(-0.0694916293183465,0.,-0.997582534658001)) ;
#16912 = DIRECTION('',(-0.0694916293183465,0.,-0.997582534658001)) ;
#16913 = DIRECTION('',(0.,1.,0.)) ;
#16914 = DIRECTION('',(0.0694916293183465,0.,0.997582534658001)) ;
#16915 = DIRECTION('center_axis',(0.997582534658001,0.,-0.0694916293183465)) ;
#16916 = DIRECTION('ref_axis',(-0.0694916293183465,0.,-0.997582534658001)) ;
#16917 = DIRECTION('',(0.0694916293183465,0.,0.997582534658001)) ;
#16918 = DIRECTION('',(0.,-1.,0.)) ;
#16919 = DIRECTION('',(-0.0694916293183465,0.,-0.997582534658001)) ;
#16920 = DIRECTION('center_axis',(-0.0694916293183465,0.,-0.997582534658001)) ;
#16921 = DIRECTION('ref_axis',(-0.997582534658001,0.,0.0694916293183465)) ;
#16922 = DIRECTION('',(-0.997582534658001,0.,0.0694916293183465)) ;
#16923 = DIRECTION('',(0.,1.,0.)) ;
#16924 = DIRECTION('',(-0.997582534658001,0.,0.0694916293183465)) ;
#16925 = DIRECTION('center_axis',(0.,-1.,0.)) ;
#16926 = DIRECTION('ref_axis',(-0.997582534658001,0.,0.0694916293183465)) ;
#16927 = DIRECTION('',(-0.997582534658001,0.,0.0694916293183465)) ;
#16928 = DIRECTION('',(-0.997582534658001,0.,0.0694916293183465)) ;
#16929 = DIRECTION('',(-0.0694916293183465,0.,-0.997582534658001)) ;
#16930 = DIRECTION('',(-0.0694916293183465,0.,-0.997582534658001)) ;
#16931 = DIRECTION('center_axis',(0.997582534658001,0.,-0.0694916293183465)) ;
#16932 = DIRECTION('ref_axis',(-0.0694916293183465,0.,-0.997582534658001)) ;
#16933 = DIRECTION('',(0.0694916293183465,0.,0.997582534658001)) ;
#16934 = DIRECTION('center_axis',(0.997582534658001,0.,-0.0694916293183465)) ;
#16935 = DIRECTION('ref_axis',(-0.0694916293183465,0.,-0.997582534658001)) ;
#16936 = DIRECTION('',(0.,-1.,0.)) ;
#16937 = DIRECTION('',(0.0694916293183465,0.,0.997582534658001)) ;
#16938 = DIRECTION('center_axis',(0.,1.,0.)) ;
#16939 = DIRECTION('ref_axis',(0.997582534658001,0.,-0.0694916293183465)) ;
#16940 = DIRECTION('',(-0.997582534658001,0.,0.0694916293183465)) ;
#16941 = DIRECTION('',(-0.997582534658001,0.,0.0694916293183465)) ;
#16942 = DIRECTION('center_axis',(-0.0694916293183465,0.,-0.997582534658001)) ;
#16943 = DIRECTION('ref_axis',(-0.997582534658001,0.,0.0694916293183465)) ;
#16944 = DIRECTION('center_axis',(0.0694916293183465,0.,0.997582534658001)) ;
#16945 = DIRECTION('ref_axis',(0.997582534658001,0.,-0.0694916293183465)) ;
#16946 = DIRECTION('axis',(0.,0.,1.)) ;
#16947 = DIRECTION('refdir',(1.,0.,0.)) ;
#16948 = DIRECTION('center_axis',(0.,1.,0.)) ;
#16949 = DIRECTION('ref_axis',(1.,0.,0.)) ;
#16950 = DIRECTION('center_axis',(0.,1.,0.)) ;
#16951 = DIRECTION('ref_axis',(1.,0.,0.)) ;
#16952 = DIRECTION('',(0.,-1.,0.)) ;
#16953 = DIRECTION('center_axis',(0.,-1.,0.)) ;
#16954 = DIRECTION('ref_axis',(1.,0.,0.)) ;
#16955 = DIRECTION('center_axis',(0.,-1.,0.)) ;
#16956 = DIRECTION('ref_axis',(-1.,0.,0.)) ;
#16957 = DIRECTION('center_axis',(0.,1.,0.)) ;
#16958 = DIRECTION('ref_axis',(1.,0.,0.)) ;
#16959 = DIRECTION('axis',(0.,0.,1.)) ;
#16960 = DIRECTION('refdir',(1.,0.,0.)) ;
#16961 = DIRECTION('center_axis',(0.,0.,1.)) ;
#16962 = DIRECTION('ref_axis',(1.,0.,0.)) ;
#16963 = DIRECTION('center_axis',(-0.382084887170903,-0.0559079744467157,
0.922434516585792)) ;
#16964 = DIRECTION('ref_axis',(0.924127230956646,-0.0231154232803137,0.381385026201834)) ;
#16965 = DIRECTION('center_axis',(0.922434516585794,0.0559079744467152,-0.382084887170899)) ;
#16966 = DIRECTION('ref_axis',(0.386153547971701,-0.13355165491274,0.912715395322625)) ;
#16967 = DIRECTION('center_axis',(0.,0.,1.)) ;
#16968 = DIRECTION('ref_axis',(1.,0.,0.)) ;
#16969 = DIRECTION('center_axis',(-0.922434516585794,-0.0559079744467152,
0.382084887170899)) ;
#16970 = DIRECTION('ref_axis',(0.386153547971701,-0.13355165491274,0.912715395322625)) ;
#16971 = DIRECTION('center_axis',(0.922434516585793,0.0559079744467158,0.3820848871709)) ;
#16972 = DIRECTION('ref_axis',(0.386153547971702,-0.13355165491274,-0.912715395322624)) ;
#16973 = DIRECTION('center_axis',(0.922434516585793,0.0559079744467158,0.3820848871709)) ;
#16974 = DIRECTION('ref_axis',(0.386153547971702,-0.13355165491274,-0.912715395322624)) ;
#16975 = DIRECTION('center_axis',(0.,-1.,0.)) ;
#16976 = DIRECTION('ref_axis',(-1.,0.,0.)) ;
#16977 = DIRECTION('center_axis',(0.922434516585793,0.0559079744467158,0.3820848871709)) ;
#16978 = DIRECTION('ref_axis',(0.386153547971702,-0.13355165491274,-0.912715395322624)) ;
#16979 = DIRECTION('center_axis',(0.,0.,1.)) ;
#16980 = DIRECTION('ref_axis',(-0.999082895817669,-0.0428178383921971,0.)) ;
#16981 = DIRECTION('center_axis',(-0.922434516585793,-0.0559079744467158,
-0.3820848871709)) ;
#16982 = DIRECTION('ref_axis',(0.386153547971702,-0.13355165491274,-0.912715395322624)) ;
#16983 = DIRECTION('center_axis',(-0.922434516585793,-0.0559079744467158,
-0.3820848871709)) ;
#16984 = DIRECTION('ref_axis',(0.386153547971702,-0.13355165491274,-0.912715395322624)) ;
#16985 = DIRECTION('center_axis',(0.382084887170903,0.0559079744467153,0.922434516585792)) ;
#16986 = DIRECTION('ref_axis',(0.924127230956646,-0.0231154232803136,-0.381385026201834)) ;
#16987 = DIRECTION('center_axis',(0.382084887170903,0.0559079744467153,0.922434516585792)) ;
#16988 = DIRECTION('ref_axis',(0.924127230956646,-0.0231154232803136,-0.381385026201834)) ;
#16989 = DIRECTION('center_axis',(0.,0.,1.)) ;
#16990 = DIRECTION('ref_axis',(-1.,0.,0.)) ;
#16991 = DIRECTION('center_axis',(-0.382084887170903,-0.0559079744467153,
-0.922434516585792)) ;
#16992 = DIRECTION('ref_axis',(0.924127230956646,-0.0231154232803136,-0.381385026201834)) ;
#16993 = DIRECTION('center_axis',(-0.382084887170903,-0.0559079744467153,
-0.922434516585792)) ;
#16994 = DIRECTION('ref_axis',(0.924127230956646,-0.0231154232803136,-0.381385026201834)) ;
#16995 = DIRECTION('center_axis',(-0.382084887170908,0.0559079744467156,0.92243451658579)) ;
#16996 = DIRECTION('ref_axis',(0.924127230956644,0.023115423280314,0.381385026201839)) ;
#16997 = DIRECTION('center_axis',(-0.382084887170908,0.0559079744467156,0.92243451658579)) ;
#16998 = DIRECTION('ref_axis',(0.924127230956644,0.023115423280314,0.381385026201839)) ;
#16999 = DIRECTION('center_axis',(0.,0.,1.)) ;
#17000 = DIRECTION('ref_axis',(-0.99908289581767,0.0428178383921882,0.)) ;
#17001 = DIRECTION('center_axis',(0.382084887170908,-0.0559079744467156,-0.92243451658579)) ;
#17002 = DIRECTION('ref_axis',(0.924127230956644,0.023115423280314,0.381385026201839)) ;
#17003 = DIRECTION('center_axis',(0.382084887170908,-0.0559079744467156,-0.92243451658579)) ;
#17004 = DIRECTION('ref_axis',(0.924127230956644,0.023115423280314,0.381385026201839)) ;
#17005 = DIRECTION('center_axis',(-0.922434516585791,0.0559079744467153,0.382084887170906)) ;
#17006 = DIRECTION('ref_axis',(0.386153547971708,0.133551654912737,0.912715395322622)) ;
#17007 = DIRECTION('center_axis',(-0.922434516585791,0.0559079744467153,0.382084887170906)) ;
#17008 = DIRECTION('ref_axis',(0.386153547971708,0.133551654912737,0.912715395322622)) ;
#17009 = DIRECTION('center_axis',(0.,0.,1.)) ;
#17010 = DIRECTION('ref_axis',(1.,0.,0.)) ;
#17011 = DIRECTION('center_axis',(0.922434516585791,-0.0559079744467153,-0.382084887170906)) ;
#17012 = DIRECTION('ref_axis',(0.386153547971708,0.133551654912737,0.912715395322622)) ;
#17013 = DIRECTION('center_axis',(0.922434516585791,-0.0559079744467153,-0.382084887170906)) ;
#17014 = DIRECTION('ref_axis',(0.386153547971708,0.133551654912737,0.912715395322622)) ;
#17015 = DIRECTION('center_axis',(0.,-1.,0.)) ;
#17016 = DIRECTION('ref_axis',(-1.,0.,0.)) ;
#17017 = DIRECTION('center_axis',(0.922434516585791,-0.0559079744467153,-0.382084887170906)) ;
#17018 = DIRECTION('ref_axis',(0.386153547971708,0.133551654912737,0.912715395322622)) ;
#17019 = DIRECTION('center_axis',(-0.922434516585791,0.0559079744467157,-0.382084887170905)) ;
#17020 = DIRECTION('ref_axis',(0.386153547971708,0.133551654912738,-0.912715395322622)) ;
#17021 = DIRECTION('center_axis',(0.,0.,1.)) ;
#17022 = DIRECTION('ref_axis',(1.,0.,0.)) ;
#17023 = DIRECTION('center_axis',(0.922434516585791,-0.0559079744467157,0.382084887170905)) ;
#17024 = DIRECTION('ref_axis',(0.386153547971708,0.133551654912738,-0.912715395322622)) ;
#17025 = DIRECTION('center_axis',(-0.382084887170906,0.0559079744467161,-0.922434516585791)) ;
#17026 = DIRECTION('ref_axis',(0.924127230956645,0.023115423280314,-0.381385026201837)) ;
#17027 = DIRECTION('center_axis',(0.,0.,1.)) ;
#17028 = DIRECTION('ref_axis',(1.,0.,0.)) ;
#17029 = DIRECTION('center_axis',(0.382084887170906,-0.0559079744467161,0.922434516585791)) ;
#17030 = DIRECTION('ref_axis',(0.924127230956645,0.023115423280314,-0.381385026201837)) ;
#17031 = DIRECTION('center_axis',(0.382084887170903,0.0559079744467153,-0.922434516585792)) ;
#17032 = DIRECTION('ref_axis',(0.924127230956646,-0.0231154232803136,0.381385026201834)) ;
#17033 = DIRECTION('center_axis',(0.,0.,1.)) ;
#17034 = DIRECTION('ref_axis',(1.,0.,0.)) ;
#17035 = DIRECTION('center_axis',(-0.382084887170903,-0.0559079744467153,
0.922434516585792)) ;
#17036 = DIRECTION('ref_axis',(0.924127230956646,-0.0231154232803136,0.381385026201834)) ;
#17037 = DIRECTION('center_axis',(0.922434516585794,0.0559079744467152,-0.382084887170899)) ;
#17038 = DIRECTION('ref_axis',(0.386153547971701,-0.13355165491274,0.912715395322625)) ;
#17039 = DIRECTION('center_axis',(0.,0.,1.)) ;
#17040 = DIRECTION('ref_axis',(1.,0.,0.)) ;
#17041 = DIRECTION('center_axis',(-0.922434516585794,-0.0559079744467152,
0.382084887170899)) ;
#17042 = DIRECTION('ref_axis',(0.386153547971701,-0.13355165491274,0.912715395322625)) ;
#17043 = DIRECTION('center_axis',(0.922434516585793,0.0559079744467158,0.3820848871709)) ;
#17044 = DIRECTION('ref_axis',(0.386153547971702,-0.13355165491274,-0.912715395322624)) ;
#17045 = DIRECTION('center_axis',(0.922434516585793,0.0559079744467158,0.3820848871709)) ;
#17046 = DIRECTION('ref_axis',(0.386153547971702,-0.13355165491274,-0.912715395322624)) ;
#17047 = DIRECTION('center_axis',(0.,-1.,0.)) ;
#17048 = DIRECTION('ref_axis',(-1.,0.,0.)) ;
#17049 = DIRECTION('center_axis',(0.922434516585793,0.0559079744467158,0.3820848871709)) ;
#17050 = DIRECTION('ref_axis',(0.386153547971702,-0.13355165491274,-0.912715395322624)) ;
#17051 = DIRECTION('center_axis',(0.,0.,1.)) ;
#17052 = DIRECTION('ref_axis',(-0.999082895817669,-0.0428178383921971,0.)) ;
#17053 = DIRECTION('center_axis',(-0.922434516585793,-0.0559079744467158,
-0.3820848871709)) ;
#17054 = DIRECTION('ref_axis',(0.386153547971702,-0.13355165491274,-0.912715395322624)) ;
#17055 = DIRECTION('center_axis',(-0.922434516585793,-0.0559079744467158,
-0.3820848871709)) ;
#17056 = DIRECTION('ref_axis',(0.386153547971702,-0.13355165491274,-0.912715395322624)) ;
#17057 = DIRECTION('center_axis',(0.382084887170903,0.0559079744467153,0.922434516585792)) ;
#17058 = DIRECTION('ref_axis',(0.924127230956646,-0.0231154232803136,-0.381385026201834)) ;
#17059 = DIRECTION('center_axis',(0.382084887170903,0.0559079744467153,0.922434516585792)) ;
#17060 = DIRECTION('ref_axis',(0.924127230956646,-0.0231154232803136,-0.381385026201834)) ;
#17061 = DIRECTION('center_axis',(0.,0.,1.)) ;
#17062 = DIRECTION('ref_axis',(-1.,0.,0.)) ;
#17063 = DIRECTION('center_axis',(-0.382084887170903,-0.0559079744467153,
-0.922434516585792)) ;
#17064 = DIRECTION('ref_axis',(0.924127230956646,-0.0231154232803136,-0.381385026201834)) ;
#17065 = DIRECTION('center_axis',(-0.382084887170903,-0.0559079744467153,
-0.922434516585792)) ;
#17066 = DIRECTION('ref_axis',(0.924127230956646,-0.0231154232803136,-0.381385026201834)) ;
#17067 = DIRECTION('center_axis',(-0.382084887170908,0.0559079744467156,0.92243451658579)) ;
#17068 = DIRECTION('ref_axis',(0.924127230956644,0.023115423280314,0.381385026201839)) ;
#17069 = DIRECTION('center_axis',(-0.382084887170908,0.0559079744467156,0.92243451658579)) ;
#17070 = DIRECTION('ref_axis',(0.924127230956644,0.023115423280314,0.381385026201839)) ;
#17071 = DIRECTION('center_axis',(0.,0.,1.)) ;
#17072 = DIRECTION('ref_axis',(-0.99908289581767,0.0428178383921882,0.)) ;
#17073 = DIRECTION('center_axis',(0.382084887170908,-0.0559079744467156,-0.92243451658579)) ;
#17074 = DIRECTION('ref_axis',(0.924127230956644,0.023115423280314,0.381385026201839)) ;
#17075 = DIRECTION('center_axis',(0.382084887170908,-0.0559079744467156,-0.92243451658579)) ;
#17076 = DIRECTION('ref_axis',(0.924127230956644,0.023115423280314,0.381385026201839)) ;
#17077 = DIRECTION('center_axis',(-0.922434516585791,0.0559079744467157,0.382084887170905)) ;
#17078 = DIRECTION('ref_axis',(0.386153547971708,0.133551654912738,0.912715395322622)) ;
#17079 = DIRECTION('center_axis',(-0.922434516585791,0.0559079744467157,0.382084887170905)) ;
#17080 = DIRECTION('ref_axis',(0.386153547971708,0.133551654912738,0.912715395322622)) ;
#17081 = DIRECTION('center_axis',(0.,0.,1.)) ;
#17082 = DIRECTION('ref_axis',(1.,0.,0.)) ;
#17083 = DIRECTION('center_axis',(0.922434516585791,-0.0559079744467157,-0.382084887170905)) ;
#17084 = DIRECTION('ref_axis',(0.386153547971708,0.133551654912738,0.912715395322622)) ;
#17085 = DIRECTION('center_axis',(0.922434516585791,-0.0559079744467157,-0.382084887170905)) ;
#17086 = DIRECTION('ref_axis',(0.386153547971708,0.133551654912738,0.912715395322622)) ;
#17087 = DIRECTION('center_axis',(0.,-1.,0.)) ;
#17088 = DIRECTION('ref_axis',(-1.,0.,0.)) ;
#17089 = DIRECTION('center_axis',(0.922434516585791,-0.0559079744467157,-0.382084887170905)) ;
#17090 = DIRECTION('ref_axis',(0.386153547971708,0.133551654912738,0.912715395322622)) ;
#17091 = DIRECTION('center_axis',(-0.922434516585791,0.0559079744467157,-0.382084887170905)) ;
#17092 = DIRECTION('ref_axis',(0.386153547971708,0.133551654912738,-0.912715395322622)) ;
#17093 = DIRECTION('center_axis',(0.,0.,1.)) ;
#17094 = DIRECTION('ref_axis',(1.,0.,0.)) ;
#17095 = DIRECTION('center_axis',(0.922434516585791,-0.0559079744467157,0.382084887170905)) ;
#17096 = DIRECTION('ref_axis',(0.386153547971708,0.133551654912738,-0.912715395322622)) ;
#17097 = DIRECTION('center_axis',(-0.382084887170905,0.0559079744467153,-0.922434516585791)) ;
#17098 = DIRECTION('ref_axis',(0.924127230956645,0.0231154232803137,-0.381385026201837)) ;
#17099 = DIRECTION('center_axis',(0.,0.,1.)) ;
#17100 = DIRECTION('ref_axis',(1.,0.,0.)) ;
#17101 = DIRECTION('center_axis',(0.382084887170905,-0.0559079744467153,0.922434516585791)) ;
#17102 = DIRECTION('ref_axis',(0.924127230956645,0.0231154232803137,-0.381385026201837)) ;
#17103 = DIRECTION('center_axis',(0.382084887170903,0.0559079744467153,-0.922434516585792)) ;
#17104 = DIRECTION('ref_axis',(0.924127230956646,-0.0231154232803136,0.381385026201834)) ;
#17105 = DIRECTION('center_axis',(0.,0.,1.)) ;
#17106 = DIRECTION('ref_axis',(1.,0.,0.)) ;
#17107 = DIRECTION('center_axis',(-0.382084887170903,-0.0559079744467153,
0.922434516585792)) ;
#17108 = DIRECTION('ref_axis',(0.924127230956646,-0.0231154232803136,0.381385026201834)) ;
#17109 = DIRECTION('center_axis',(0.922434516585793,0.0559079744467162,-0.3820848871709)) ;
#17110 = DIRECTION('ref_axis',(0.386153547971703,-0.133551654912741,0.912715395322624)) ;
#17111 = DIRECTION('center_axis',(0.,0.,1.)) ;
#17112 = DIRECTION('ref_axis',(1.,0.,0.)) ;
#17113 = DIRECTION('center_axis',(-0.922434516585793,-0.0559079744467162,
0.3820848871709)) ;
#17114 = DIRECTION('ref_axis',(0.386153547971703,-0.133551654912741,0.912715395322624)) ;
#17115 = DIRECTION('center_axis',(0.922434516585794,0.0559079744467152,0.382084887170899)) ;
#17116 = DIRECTION('ref_axis',(0.386153547971701,-0.13355165491274,-0.912715395322625)) ;
#17117 = DIRECTION('center_axis',(0.922434516585794,0.0559079744467152,0.382084887170899)) ;
#17118 = DIRECTION('ref_axis',(0.386153547971701,-0.13355165491274,-0.912715395322625)) ;
#17119 = DIRECTION('center_axis',(0.,-1.,0.)) ;
#17120 = DIRECTION('ref_axis',(-1.,0.,0.)) ;
#17121 = DIRECTION('center_axis',(0.922434516585794,0.0559079744467152,0.382084887170899)) ;
#17122 = DIRECTION('ref_axis',(0.386153547971701,-0.13355165491274,-0.912715395322625)) ;
#17123 = DIRECTION('center_axis',(0.,0.,1.)) ;
#17124 = DIRECTION('ref_axis',(-0.99908289581767,-0.0428178383921882,0.)) ;
#17125 = DIRECTION('center_axis',(-0.922434516585794,-0.0559079744467152,
-0.382084887170899)) ;
#17126 = DIRECTION('ref_axis',(0.386153547971701,-0.13355165491274,-0.912715395322625)) ;
#17127 = DIRECTION('center_axis',(-0.922434516585794,-0.0559079744467152,
-0.382084887170899)) ;
#17128 = DIRECTION('ref_axis',(0.386153547971701,-0.13355165491274,-0.912715395322625)) ;
#17129 = DIRECTION('center_axis',(0.382084887170903,0.0559079744467153,0.922434516585792)) ;
#17130 = DIRECTION('ref_axis',(0.924127230956646,-0.0231154232803136,-0.381385026201834)) ;
#17131 = DIRECTION('center_axis',(0.382084887170903,0.0559079744467153,0.922434516585792)) ;
#17132 = DIRECTION('ref_axis',(0.924127230956646,-0.0231154232803136,-0.381385026201834)) ;
#17133 = DIRECTION('center_axis',(0.,0.,1.)) ;
#17134 = DIRECTION('ref_axis',(-1.,0.,0.)) ;
#17135 = DIRECTION('center_axis',(-0.382084887170903,-0.0559079744467153,
-0.922434516585792)) ;
#17136 = DIRECTION('ref_axis',(0.924127230956646,-0.0231154232803136,-0.381385026201834)) ;
#17137 = DIRECTION('center_axis',(-0.382084887170903,-0.0559079744467153,
-0.922434516585792)) ;
#17138 = DIRECTION('ref_axis',(0.924127230956646,-0.0231154232803136,-0.381385026201834)) ;
#17139 = DIRECTION('center_axis',(-0.382084887170908,0.0559079744467156,0.92243451658579)) ;
#17140 = DIRECTION('ref_axis',(0.924127230956644,0.023115423280314,0.381385026201839)) ;
#17141 = DIRECTION('center_axis',(-0.382084887170908,0.0559079744467156,0.92243451658579)) ;
#17142 = DIRECTION('ref_axis',(0.924127230956644,0.023115423280314,0.381385026201839)) ;
#17143 = DIRECTION('center_axis',(0.,0.,1.)) ;
#17144 = DIRECTION('ref_axis',(-0.99908289581767,0.0428178383921882,0.)) ;
#17145 = DIRECTION('center_axis',(0.382084887170908,-0.0559079744467156,-0.92243451658579)) ;
#17146 = DIRECTION('ref_axis',(0.924127230956644,0.023115423280314,0.381385026201839)) ;
#17147 = DIRECTION('center_axis',(0.382084887170908,-0.0559079744467156,-0.92243451658579)) ;
#17148 = DIRECTION('ref_axis',(0.924127230956644,0.023115423280314,0.381385026201839)) ;
#17149 = DIRECTION('center_axis',(-0.922434516585791,0.0559079744467157,0.382084887170905)) ;
#17150 = DIRECTION('ref_axis',(0.386153547971708,0.133551654912738,0.912715395322622)) ;
#17151 = DIRECTION('center_axis',(-0.922434516585791,0.0559079744467157,0.382084887170905)) ;
#17152 = DIRECTION('ref_axis',(0.386153547971708,0.133551654912738,0.912715395322622)) ;
#17153 = DIRECTION('center_axis',(0.,0.,1.)) ;
#17154 = DIRECTION('ref_axis',(1.,0.,0.)) ;
#17155 = DIRECTION('center_axis',(0.922434516585791,-0.0559079744467157,-0.382084887170905)) ;
#17156 = DIRECTION('ref_axis',(0.386153547971708,0.133551654912738,0.912715395322622)) ;
#17157 = DIRECTION('center_axis',(0.922434516585791,-0.0559079744467157,-0.382084887170905)) ;
#17158 = DIRECTION('ref_axis',(0.386153547971708,0.133551654912738,0.912715395322622)) ;
#17159 = DIRECTION('center_axis',(0.,-1.,0.)) ;
#17160 = DIRECTION('ref_axis',(-1.,0.,0.)) ;
#17161 = DIRECTION('center_axis',(0.922434516585791,-0.0559079744467157,-0.382084887170905)) ;
#17162 = DIRECTION('ref_axis',(0.386153547971708,0.133551654912738,0.912715395322622)) ;
#17163 = DIRECTION('center_axis',(-0.922434516585791,0.0559079744467157,-0.382084887170905)) ;
#17164 = DIRECTION('ref_axis',(0.386153547971708,0.133551654912738,-0.912715395322622)) ;
#17165 = DIRECTION('center_axis',(0.,0.,1.)) ;
#17166 = DIRECTION('ref_axis',(1.,0.,0.)) ;
#17167 = DIRECTION('center_axis',(0.922434516585791,-0.0559079744467157,0.382084887170905)) ;
#17168 = DIRECTION('ref_axis',(0.386153547971708,0.133551654912738,-0.912715395322622)) ;
#17169 = DIRECTION('center_axis',(-0.382084887170906,0.0559079744467155,-0.922434516585791)) ;
#17170 = DIRECTION('ref_axis',(0.924127230956645,0.0231154232803138,-0.381385026201837)) ;
#17171 = DIRECTION('center_axis',(0.,0.,1.)) ;
#17172 = DIRECTION('ref_axis',(1.,0.,0.)) ;
#17173 = DIRECTION('center_axis',(0.382084887170906,-0.0559079744467155,0.922434516585791)) ;
#17174 = DIRECTION('ref_axis',(0.924127230956645,0.0231154232803138,-0.381385026201837)) ;
#17175 = DIRECTION('center_axis',(0.382084887170903,0.0559079744467153,-0.922434516585792)) ;
#17176 = DIRECTION('ref_axis',(0.924127230956646,-0.0231154232803136,0.381385026201834)) ;
#17177 = DIRECTION('center_axis',(0.,0.,1.)) ;
#17178 = DIRECTION('ref_axis',(1.,0.,0.)) ;
#17179 = DIRECTION('center_axis',(-0.382084887170903,-0.0559079744467153,
0.922434516585792)) ;
#17180 = DIRECTION('ref_axis',(0.924127230956646,-0.0231154232803136,0.381385026201834)) ;
#17181 = DIRECTION('center_axis',(0.922434516585793,0.0559079744467156,-0.3820848871709)) ;
#17182 = DIRECTION('ref_axis',(0.386153547971702,-0.13355165491274,0.912715395322624)) ;
#17183 = DIRECTION('center_axis',(0.,0.,1.)) ;
#17184 = DIRECTION('ref_axis',(1.,0.,0.)) ;
#17185 = DIRECTION('center_axis',(-0.922434516585793,-0.0559079744467156,
0.3820848871709)) ;
#17186 = DIRECTION('ref_axis',(0.386153547971702,-0.13355165491274,0.912715395322624)) ;
#17187 = DIRECTION('center_axis',(0.922434516585794,0.0559079744467156,0.382084887170899)) ;
#17188 = DIRECTION('ref_axis',(0.386153547971701,-0.133551654912741,-0.912715395322625)) ;
#17189 = DIRECTION('center_axis',(0.922434516585794,0.0559079744467156,0.382084887170899)) ;
#17190 = DIRECTION('ref_axis',(0.386153547971701,-0.133551654912741,-0.912715395322625)) ;
#17191 = DIRECTION('center_axis',(0.,-1.,0.)) ;
#17192 = DIRECTION('ref_axis',(-1.,0.,0.)) ;
#17193 = DIRECTION('center_axis',(0.922434516585794,0.0559079744467156,0.382084887170899)) ;
#17194 = DIRECTION('ref_axis',(0.386153547971701,-0.133551654912741,-0.912715395322625)) ;
#17195 = DIRECTION('center_axis',(0.,0.,1.)) ;
#17196 = DIRECTION('ref_axis',(-0.99908289581767,-0.0428178383921882,0.)) ;
#17197 = DIRECTION('center_axis',(-0.922434516585794,-0.0559079744467156,
-0.382084887170899)) ;
#17198 = DIRECTION('ref_axis',(0.386153547971701,-0.133551654912741,-0.912715395322625)) ;
#17199 = DIRECTION('center_axis',(-0.922434516585794,-0.0559079744467156,
-0.382084887170899)) ;
#17200 = DIRECTION('ref_axis',(0.386153547971701,-0.133551654912741,-0.912715395322625)) ;
#17201 = DIRECTION('center_axis',(0.382084887170903,0.0559079744467155,0.922434516585792)) ;
#17202 = DIRECTION('ref_axis',(0.924127230956646,-0.0231154232803136,-0.381385026201834)) ;
#17203 = DIRECTION('center_axis',(0.382084887170903,0.0559079744467155,0.922434516585792)) ;
#17204 = DIRECTION('ref_axis',(0.924127230956646,-0.0231154232803136,-0.381385026201834)) ;
#17205 = DIRECTION('center_axis',(0.,0.,1.)) ;
#17206 = DIRECTION('ref_axis',(-1.,8.88178419700128E-15,0.)) ;
#17207 = DIRECTION('center_axis',(-0.382084887170903,-0.0559079744467155,
-0.922434516585792)) ;
#17208 = DIRECTION('ref_axis',(0.924127230956646,-0.0231154232803136,-0.381385026201834)) ;
#17209 = DIRECTION('center_axis',(-0.382084887170903,-0.0559079744467155,
-0.922434516585792)) ;
#17210 = DIRECTION('ref_axis',(0.924127230956646,-0.0231154232803136,-0.381385026201834)) ;
#17211 = DIRECTION('center_axis',(-0.382084887170906,0.0559079744467155,0.922434516585791)) ;
#17212 = DIRECTION('ref_axis',(0.924127230956645,0.0231154232803138,0.381385026201837)) ;
#17213 = DIRECTION('center_axis',(-0.382084887170906,0.0559079744467155,0.922434516585791)) ;
#17214 = DIRECTION('ref_axis',(0.924127230956645,0.0231154232803138,0.381385026201837)) ;
#17215 = DIRECTION('center_axis',(0.,0.,1.)) ;
#17216 = DIRECTION('ref_axis',(-0.99908289581767,0.0428178383921793,0.)) ;
#17217 = DIRECTION('center_axis',(0.382084887170906,-0.0559079744467155,-0.922434516585791)) ;
#17218 = DIRECTION('ref_axis',(0.924127230956645,0.0231154232803138,0.381385026201837)) ;
#17219 = DIRECTION('center_axis',(0.382084887170906,-0.0559079744467155,-0.922434516585791)) ;
#17220 = DIRECTION('ref_axis',(0.924127230956645,0.0231154232803138,0.381385026201837)) ;
#17221 = DIRECTION('center_axis',(-0.922434516585792,0.0559079744467155,0.382084887170904)) ;
#17222 = DIRECTION('ref_axis',(0.386153547971707,0.133551654912738,0.912715395322623)) ;
#17223 = DIRECTION('center_axis',(-0.922434516585792,0.0559079744467155,0.382084887170904)) ;
#17224 = DIRECTION('ref_axis',(0.386153547971707,0.133551654912738,0.912715395322623)) ;
#17225 = DIRECTION('center_axis',(0.,0.,1.)) ;
#17226 = DIRECTION('ref_axis',(1.,0.,0.)) ;
#17227 = DIRECTION('center_axis',(0.922434516585792,-0.0559079744467155,-0.382084887170904)) ;
#17228 = DIRECTION('ref_axis',(0.386153547971707,0.133551654912738,0.912715395322623)) ;
#17229 = DIRECTION('center_axis',(0.922434516585792,-0.0559079744467155,-0.382084887170904)) ;
#17230 = DIRECTION('ref_axis',(0.386153547971707,0.133551654912738,0.912715395322623)) ;
#17231 = DIRECTION('center_axis',(0.,-1.,0.)) ;
#17232 = DIRECTION('ref_axis',(-1.,0.,0.)) ;
#17233 = DIRECTION('center_axis',(0.922434516585792,-0.0559079744467155,-0.382084887170904)) ;
#17234 = DIRECTION('ref_axis',(0.386153547971707,0.133551654912738,0.912715395322623)) ;
#17235 = DIRECTION('center_axis',(-0.922434516585791,0.0559079744467157,-0.382084887170905)) ;
#17236 = DIRECTION('ref_axis',(0.386153547971708,0.133551654912738,-0.912715395322622)) ;
#17237 = DIRECTION('center_axis',(0.,0.,1.)) ;
#17238 = DIRECTION('ref_axis',(1.,0.,0.)) ;
#17239 = DIRECTION('center_axis',(0.922434516585791,-0.0559079744467157,0.382084887170905)) ;
#17240 = DIRECTION('ref_axis',(0.386153547971708,0.133551654912738,-0.912715395322622)) ;
#17241 = DIRECTION('center_axis',(-0.382084887170906,0.0559079744467155,-0.922434516585791)) ;
#17242 = DIRECTION('ref_axis',(0.924127230956645,0.0231154232803138,-0.381385026201837)) ;
#17243 = DIRECTION('center_axis',(0.382084887170903,0.0559079744467157,-0.922434516585792)) ;
#17244 = DIRECTION('ref_axis',(0.924127230956646,-0.0231154232803137,0.381385026201834)) ;
#17245 = DIRECTION('center_axis',(0.382084887170903,0.0559079744467157,-0.922434516585792)) ;
#17246 = DIRECTION('ref_axis',(0.924127230956646,-0.0231154232803137,0.381385026201834)) ;
#17247 = DIRECTION('',(-0.382084887170903,-0.0559079744467157,0.922434516585792)) ;
#17248 = DIRECTION('center_axis',(-0.705811580947695,-0.0604981355097965,
0.705811580947745)) ;
#17249 = DIRECTION('ref_axis',(0.707106781186573,-1.76822503816994E-14,0.707106781186522)) ;
#17250 = DIRECTION('center_axis',(-0.705811580947695,-0.0604981355097965,
0.705811580947745)) ;
#17251 = DIRECTION('ref_axis',(0.707106781186573,-1.76822503816994E-14,0.707106781186522)) ;
#17252 = DIRECTION('center_axis',(-0.705811580947695,-0.0604981355097965,
0.705811580947745)) ;
#17253 = DIRECTION('ref_axis',(0.707106781186573,-1.76822503816994E-14,0.707106781186522)) ;
#17254 = DIRECTION('center_axis',(0.382084887170903,0.0559079744467157,-0.922434516585792)) ;
#17255 = DIRECTION('ref_axis',(0.924127230956646,-0.0231154232803137,0.381385026201834)) ;
#17256 = DIRECTION('center_axis',(0.922434516585794,0.0559079744467152,-0.382084887170899)) ;
#17257 = DIRECTION('ref_axis',(0.386153547971701,-0.13355165491274,0.912715395322625)) ;
#17258 = DIRECTION('',(-0.922434516585794,-0.0559079744467152,0.382084887170899)) ;
#17259 = DIRECTION('center_axis',(-0.99816831025626,-0.0604981355098033,-1.24140640981796E-16)) ;
#17260 = DIRECTION('ref_axis',(-3.40659855495112E-17,-1.13820469365426E-15,
1.)) ;
#17261 = DIRECTION('center_axis',(-0.99816831025626,-0.0604981355098033,-1.24140640981796E-16)) ;
#17262 = DIRECTION('ref_axis',(-3.40659855495112E-17,-1.13820469365426E-15,
1.)) ;
#17263 = DIRECTION('center_axis',(0.922434516585793,0.0559079744467158,0.3820848871709)) ;
#17264 = DIRECTION('ref_axis',(0.386153547971702,-0.13355165491274,-0.912715395322624)) ;
#17265 = DIRECTION('',(-0.922434516585793,-0.0559079744467158,-0.3820848871709)) ;
#17266 = DIRECTION('center_axis',(-0.705811580947751,-0.0604981355097965,
-0.705811580947687)) ;
#17267 = DIRECTION('ref_axis',(0.707106781186515,1.77143124857461E-14,-0.70710678118658)) ;
#17268 = DIRECTION('center_axis',(0.382084887170903,0.0559079744467153,0.922434516585792)) ;
#17269 = DIRECTION('ref_axis',(0.924127230956646,-0.0231154232803136,-0.381385026201834)) ;
#17270 = DIRECTION('',(-0.382084887170903,-0.0559079744467153,-0.922434516585792)) ;
#17271 = DIRECTION('center_axis',(3.28955978897023E-14,-0.0604981355098033,
-0.99816831025626)) ;
#17272 = DIRECTION('ref_axis',(1.,1.99586597690074E-15,3.28957187518098E-14)) ;
#17273 = DIRECTION('center_axis',(-0.382084887170908,0.0559079744467156,0.92243451658579)) ;
#17274 = DIRECTION('ref_axis',(0.924127230956644,0.023115423280314,0.381385026201839)) ;
#17275 = DIRECTION('',(0.382084887170908,-0.0559079744467156,-0.92243451658579)) ;
#17276 = DIRECTION('center_axis',(0.705811580947711,-0.0604981355097965,-0.705811580947728)) ;
#17277 = DIRECTION('ref_axis',(0.707106781186557,1.85078495608992E-14,0.707106781186538)) ;
#17278 = DIRECTION('center_axis',(-0.922434516585791,0.0559079744467153,0.382084887170906)) ;
#17279 = DIRECTION('ref_axis',(0.386153547971708,0.133551654912737,0.912715395322622)) ;
#17280 = DIRECTION('',(0.922434516585791,-0.0559079744467153,-0.382084887170905)) ;
#17281 = DIRECTION('center_axis',(0.99816831025626,-0.0604981355098033,-3.28955978897028E-14)) ;
#17282 = DIRECTION('ref_axis',(3.29408060856262E-14,2.08403676302894E-16,
1.)) ;
#17283 = DIRECTION('center_axis',(0.99816831025626,-0.0604981355098033,-3.28955978897028E-14)) ;
#17284 = DIRECTION('ref_axis',(3.29408060856262E-14,2.08403676302894E-16,
1.)) ;
#17285 = DIRECTION('center_axis',(-0.922434516585791,0.0559079744467157,-0.382084887170905)) ;
#17286 = DIRECTION('ref_axis',(0.386153547971708,0.133551654912738,-0.912715395322622)) ;
#17287 = DIRECTION('',(0.922434516585791,-0.0559079744467157,0.382084887170906)) ;
#17288 = DIRECTION('center_axis',(0.705811580947752,-0.0604981355097965,0.705811580947687)) ;
#17289 = DIRECTION('ref_axis',(0.707106781186515,-1.71051325088607E-14,-0.70710678118658)) ;
#17290 = DIRECTION('center_axis',(0.705811580947752,-0.0604981355097965,0.705811580947687)) ;
#17291 = DIRECTION('ref_axis',(0.707106781186515,-1.71051325088607E-14,-0.70710678118658)) ;
#17292 = DIRECTION('center_axis',(0.705811580947752,-0.0604981355097965,0.705811580947687)) ;
#17293 = DIRECTION('ref_axis',(0.707106781186515,-1.71051325088607E-14,-0.70710678118658)) ;
#17294 = DIRECTION('center_axis',(-0.382084887170906,0.0559079744467161,-0.922434516585791)) ;
#17295 = DIRECTION('ref_axis',(0.924127230956645,0.023115423280314,-0.381385026201837)) ;
#17296 = DIRECTION('',(0.382084887170905,-0.0559079744467161,0.922434516585791)) ;
#17297 = DIRECTION('center_axis',(0.,-0.0604981355098033,0.99816831025626)) ;
#17298 = DIRECTION('ref_axis',(1.,0.,0.)) ;
#17299 = DIRECTION('center_axis',(0.,-0.0604981355098033,0.99816831025626)) ;
#17300 = DIRECTION('ref_axis',(1.,0.,0.)) ;
#17301 = DIRECTION('center_axis',(0.382084887170903,0.0559079744467153,-0.922434516585792)) ;
#17302 = DIRECTION('ref_axis',(0.924127230956646,-0.0231154232803136,0.381385026201834)) ;
#17303 = DIRECTION('',(-0.382084887170903,-0.0559079744467153,0.922434516585792)) ;
#17304 = DIRECTION('center_axis',(-0.705811580947711,-0.0604981355097965,
0.705811580947728)) ;
#17305 = DIRECTION('ref_axis',(0.707106781186557,-1.80750111562701E-14,0.707106781186538)) ;
#17306 = DIRECTION('center_axis',(-0.705811580947711,-0.0604981355097965,
0.705811580947728)) ;
#17307 = DIRECTION('ref_axis',(0.707106781186557,-1.80750111562701E-14,0.707106781186538)) ;
#17308 = DIRECTION('center_axis',(-0.705811580947711,-0.0604981355097965,
0.705811580947728)) ;
#17309 = DIRECTION('ref_axis',(0.707106781186557,-1.80750111562701E-14,0.707106781186538)) ;
#17310 = DIRECTION('center_axis',(0.922434516585794,0.0559079744467152,-0.382084887170899)) ;
#17311 = DIRECTION('ref_axis',(0.386153547971701,-0.13355165491274,0.912715395322625)) ;
#17312 = DIRECTION('',(-0.922434516585794,-0.0559079744467152,0.382084887170899)) ;
#17313 = DIRECTION('center_axis',(-0.99816831025626,-0.0604981355098033,-1.24140640981796E-16)) ;
#17314 = DIRECTION('ref_axis',(-3.40659855495112E-17,-1.13820469365426E-15,
1.)) ;
#17315 = DIRECTION('center_axis',(-0.99816831025626,-0.0604981355098033,-1.24140640981796E-16)) ;
#17316 = DIRECTION('ref_axis',(-3.40659855495112E-17,-1.13820469365426E-15,
1.)) ;
#17317 = DIRECTION('center_axis',(0.922434516585793,0.0559079744467158,0.3820848871709)) ;
#17318 = DIRECTION('ref_axis',(0.386153547971702,-0.13355165491274,-0.912715395322624)) ;
#17319 = DIRECTION('',(-0.922434516585793,-0.0559079744467158,-0.3820848871709)) ;
#17320 = DIRECTION('center_axis',(-0.705811580947751,-0.0604981355097965,
-0.705811580947687)) ;
#17321 = DIRECTION('ref_axis',(0.707106781186515,1.77143124857461E-14,-0.70710678118658)) ;
#17322 = DIRECTION('center_axis',(0.382084887170903,0.0559079744467153,0.922434516585792)) ;
#17323 = DIRECTION('ref_axis',(0.924127230956646,-0.0231154232803136,-0.381385026201834)) ;
#17324 = DIRECTION('',(-0.382084887170903,-0.0559079744467153,-0.922434516585792)) ;
#17325 = DIRECTION('center_axis',(3.28955978897023E-14,-0.0604981355098033,
-0.99816831025626)) ;
#17326 = DIRECTION('ref_axis',(1.,1.99586597690074E-15,3.28957187518098E-14)) ;
#17327 = DIRECTION('center_axis',(-0.382084887170908,0.0559079744467156,0.92243451658579)) ;
#17328 = DIRECTION('ref_axis',(0.924127230956644,0.023115423280314,0.381385026201839)) ;
#17329 = DIRECTION('',(0.382084887170908,-0.0559079744467156,-0.92243451658579)) ;
#17330 = DIRECTION('center_axis',(0.705811580947711,-0.0604981355097965,-0.705811580947728)) ;
#17331 = DIRECTION('ref_axis',(0.707106781186557,1.85078495608992E-14,0.707106781186538)) ;
#17332 = DIRECTION('center_axis',(-0.922434516585791,0.0559079744467157,0.382084887170905)) ;
#17333 = DIRECTION('ref_axis',(0.386153547971708,0.133551654912738,0.912715395322622)) ;
#17334 = DIRECTION('',(0.922434516585791,-0.0559079744467157,-0.382084887170906)) ;
#17335 = DIRECTION('center_axis',(0.99816831025626,-0.0604981355098033,-3.28955978897028E-14)) ;
#17336 = DIRECTION('ref_axis',(3.30470118052806E-14,9.13769965328074E-16,
1.)) ;
#17337 = DIRECTION('center_axis',(0.99816831025626,-0.0604981355098033,-3.28955978897028E-14)) ;
#17338 = DIRECTION('ref_axis',(3.30470118052806E-14,9.13769965328074E-16,
1.)) ;
#17339 = DIRECTION('center_axis',(-0.922434516585791,0.0559079744467157,-0.382084887170905)) ;
#17340 = DIRECTION('ref_axis',(0.386153547971708,0.133551654912738,-0.912715395322622)) ;
#17341 = DIRECTION('',(0.922434516585791,-0.0559079744467157,0.382084887170906)) ;
#17342 = DIRECTION('center_axis',(0.705811580947752,-0.0604981355097965,0.705811580947687)) ;
#17343 = DIRECTION('ref_axis',(0.707106781186515,-1.71532256649306E-14,-0.70710678118658)) ;
#17344 = DIRECTION('center_axis',(0.705811580947752,-0.0604981355097965,0.705811580947687)) ;
#17345 = DIRECTION('ref_axis',(0.707106781186515,-1.71532256649306E-14,-0.70710678118658)) ;
#17346 = DIRECTION('center_axis',(0.705811580947752,-0.0604981355097965,0.705811580947687)) ;
#17347 = DIRECTION('ref_axis',(0.707106781186515,-1.71532256649306E-14,-0.70710678118658)) ;
#17348 = DIRECTION('center_axis',(-0.382084887170905,0.0559079744467153,-0.922434516585791)) ;
#17349 = DIRECTION('ref_axis',(0.924127230956645,0.0231154232803137,-0.381385026201837)) ;
#17350 = DIRECTION('',(0.382084887170906,-0.0559079744467153,0.922434516585791)) ;
#17351 = DIRECTION('center_axis',(0.,-0.0604981355098033,0.99816831025626)) ;
#17352 = DIRECTION('ref_axis',(1.,-4.00776300582483E-18,6.41242080931973E-17)) ;
#17353 = DIRECTION('center_axis',(0.,-0.0604981355098033,0.99816831025626)) ;
#17354 = DIRECTION('ref_axis',(1.,-4.00776300582483E-18,6.41242080931973E-17)) ;
#17355 = DIRECTION('center_axis',(0.382084887170903,0.0559079744467153,-0.922434516585792)) ;
#17356 = DIRECTION('ref_axis',(0.924127230956646,-0.0231154232803136,0.381385026201834)) ;
#17357 = DIRECTION('',(-0.382084887170903,-0.0559079744467153,0.922434516585792)) ;
#17358 = DIRECTION('center_axis',(-0.705811580947719,-0.0604981355097965,
0.70581158094772)) ;
#17359 = DIRECTION('ref_axis',(0.707106781186549,-1.87883929713068E-14,0.707106781186546)) ;
#17360 = DIRECTION('center_axis',(-0.705811580947719,-0.0604981355097965,
0.70581158094772)) ;
#17361 = DIRECTION('ref_axis',(0.707106781186549,-1.87883929713068E-14,0.707106781186546)) ;
#17362 = DIRECTION('center_axis',(-0.705811580947719,-0.0604981355097965,
0.70581158094772)) ;
#17363 = DIRECTION('ref_axis',(0.707106781186549,-1.87883929713068E-14,0.707106781186546)) ;
#17364 = DIRECTION('center_axis',(0.922434516585793,0.0559079744467162,-0.3820848871709)) ;
#17365 = DIRECTION('ref_axis',(0.386153547971703,-0.133551654912741,0.912715395322624)) ;
#17366 = DIRECTION('',(-0.922434516585793,-0.0559079744467162,0.3820848871709)) ;
#17367 = DIRECTION('center_axis',(-0.99816831025626,-0.0604981355098033,-2.48281281963583E-16)) ;
#17368 = DIRECTION('ref_axis',(-3.10601632951425E-17,-4.45663246247722E-15,
1.)) ;
#17369 = DIRECTION('center_axis',(-0.99816831025626,-0.0604981355098033,-2.48281281963583E-16)) ;
#17370 = DIRECTION('ref_axis',(-3.10601632951425E-17,-4.45663246247722E-15,
1.)) ;
#17371 = DIRECTION('center_axis',(0.922434516585794,0.0559079744467152,0.382084887170899)) ;
#17372 = DIRECTION('ref_axis',(0.386153547971701,-0.13355165491274,-0.912715395322625)) ;
#17373 = DIRECTION('',(-0.922434516585794,-0.0559079744467152,-0.382084887170899)) ;
#17374 = DIRECTION('center_axis',(-0.70581158094776,-0.0604981355097965,-0.705811580947679)) ;
#17375 = DIRECTION('ref_axis',(0.707106781186506,1.55982136186706E-14,-0.707106781186589)) ;
#17376 = DIRECTION('center_axis',(0.382084887170903,0.0559079744467153,0.922434516585792)) ;
#17377 = DIRECTION('ref_axis',(0.924127230956646,-0.0231154232803136,-0.381385026201834)) ;
#17378 = DIRECTION('',(-0.382084887170903,-0.0559079744467153,-0.922434516585792)) ;
#17379 = DIRECTION('center_axis',(3.28955978897023E-14,-0.0604981355098033,
-0.99816831025626)) ;
#17380 = DIRECTION('ref_axis',(1.,1.99586597690074E-15,3.28957187518098E-14)) ;
#17381 = DIRECTION('center_axis',(-0.382084887170908,0.0559079744467156,0.92243451658579)) ;
#17382 = DIRECTION('ref_axis',(0.924127230956644,0.023115423280314,0.381385026201839)) ;
#17383 = DIRECTION('',(0.382084887170908,-0.0559079744467156,-0.92243451658579)) ;
#17384 = DIRECTION('center_axis',(0.705811580947711,-0.0604981355097965,-0.705811580947728)) ;
#17385 = DIRECTION('ref_axis',(0.707106781186557,1.85078495608992E-14,0.707106781186538)) ;
#17386 = DIRECTION('center_axis',(-0.922434516585791,0.0559079744467157,0.382084887170905)) ;
#17387 = DIRECTION('ref_axis',(0.386153547971708,0.133551654912738,0.912715395322622)) ;
#17388 = DIRECTION('',(0.922434516585791,-0.0559079744467157,-0.382084887170906)) ;
#17389 = DIRECTION('center_axis',(0.99816831025626,-0.0604981355098033,-3.28955978897028E-14)) ;
#17390 = DIRECTION('ref_axis',(3.30650467388068E-14,1.04201838151447E-15,
1.)) ;
#17391 = DIRECTION('center_axis',(0.99816831025626,-0.0604981355098033,-3.28955978897028E-14)) ;
#17392 = DIRECTION('ref_axis',(3.30650467388068E-14,1.04201838151447E-15,
1.)) ;
#17393 = DIRECTION('center_axis',(-0.922434516585791,0.0559079744467157,-0.382084887170905)) ;
#17394 = DIRECTION('ref_axis',(0.386153547971708,0.133551654912738,-0.912715395322622)) ;
#17395 = DIRECTION('',(0.922434516585791,-0.0559079744467157,0.382084887170906)) ;
#17396 = DIRECTION('center_axis',(0.70581158094776,-0.0604981355097964,0.705811580947679)) ;
#17397 = DIRECTION('ref_axis',(0.707106781186506,-1.66081698961385E-14,-0.707106781186589)) ;
#17398 = DIRECTION('center_axis',(0.70581158094776,-0.0604981355097964,0.705811580947679)) ;
#17399 = DIRECTION('ref_axis',(0.707106781186506,-1.66081698961385E-14,-0.707106781186589)) ;
#17400 = DIRECTION('center_axis',(0.70581158094776,-0.0604981355097964,0.705811580947679)) ;
#17401 = DIRECTION('ref_axis',(0.707106781186506,-1.66081698961385E-14,-0.707106781186589)) ;
#17402 = DIRECTION('center_axis',(-0.382084887170906,0.0559079744467155,-0.922434516585791)) ;
#17403 = DIRECTION('ref_axis',(0.924127230956645,0.0231154232803138,-0.381385026201837)) ;
#17404 = DIRECTION('',(0.382084887170905,-0.0559079744467155,0.922434516585791)) ;
#17405 = DIRECTION('center_axis',(-1.24140640981796E-16,-0.0604981355098033,
0.99816831025626)) ;
#17406 = DIRECTION('ref_axis',(1.,-1.20232890174745E-17,1.92372624279592E-16)) ;
#17407 = DIRECTION('center_axis',(-1.24140640981796E-16,-0.0604981355098033,
0.99816831025626)) ;
#17408 = DIRECTION('ref_axis',(1.,-1.20232890174745E-17,1.92372624279592E-16)) ;
#17409 = DIRECTION('center_axis',(0.382084887170903,0.0559079744467153,-0.922434516585792)) ;
#17410 = DIRECTION('ref_axis',(0.924127230956646,-0.0231154232803136,0.381385026201834)) ;
#17411 = DIRECTION('',(-0.382084887170903,-0.0559079744467153,0.922434516585792)) ;
#17412 = DIRECTION('center_axis',(-0.705811580947719,-0.0604981355097965,
0.70581158094772)) ;
#17413 = DIRECTION('ref_axis',(0.707106781186549,-1.88044240233301E-14,0.707106781186546)) ;
#17414 = DIRECTION('center_axis',(-0.705811580947719,-0.0604981355097965,
0.70581158094772)) ;
#17415 = DIRECTION('ref_axis',(0.707106781186549,-1.88044240233301E-14,0.707106781186546)) ;
#17416 = DIRECTION('center_axis',(-0.705811580947719,-0.0604981355097965,
0.70581158094772)) ;
#17417 = DIRECTION('ref_axis',(0.707106781186549,-1.88044240233301E-14,0.707106781186546)) ;
#17418 = DIRECTION('center_axis',(0.922434516585793,0.0559079744467156,-0.3820848871709)) ;
#17419 = DIRECTION('ref_axis',(0.386153547971702,-0.13355165491274,0.912715395322624)) ;
#17420 = DIRECTION('',(-0.922434516585793,-0.0559079744467156,0.3820848871709)) ;
#17421 = DIRECTION('center_axis',(-0.99816831025626,-0.0604981355098033,-6.20703204908959E-17)) ;
#17422 = DIRECTION('ref_axis',(9.11766083825151E-17,-2.69321673991429E-15,
1.)) ;
#17423 = DIRECTION('center_axis',(-0.99816831025626,-0.0604981355098033,-6.20703204908959E-17)) ;
#17424 = DIRECTION('ref_axis',(9.11766083825151E-17,-2.69321673991429E-15,
1.)) ;
#17425 = DIRECTION('center_axis',(0.922434516585794,0.0559079744467156,0.382084887170899)) ;
#17426 = DIRECTION('ref_axis',(0.386153547971701,-0.133551654912741,-0.912715395322625)) ;
#17427 = DIRECTION('',(-0.922434516585794,-0.0559079744467156,-0.382084887170899)) ;
#17428 = DIRECTION('center_axis',(-0.705811580947752,-0.0604981355097965,
-0.705811580947687)) ;
#17429 = DIRECTION('ref_axis',(0.707106781186514,1.71051325088607E-14,-0.707106781186581)) ;
#17430 = DIRECTION('center_axis',(0.382084887170903,0.0559079744467155,0.922434516585792)) ;
#17431 = DIRECTION('ref_axis',(0.924127230956646,-0.0231154232803136,-0.381385026201834)) ;
#17432 = DIRECTION('',(-0.382084887170903,-0.0559079744467155,-0.922434516585792)) ;
#17433 = DIRECTION('center_axis',(1.86210961472694E-16,-0.0604981355098033,
-0.99816831025626)) ;
#17434 = DIRECTION('ref_axis',(1.,8.01552601164967E-18,1.28248416186395E-16)) ;
#17435 = DIRECTION('center_axis',(-0.382084887170906,0.0559079744467155,0.922434516585791)) ;
#17436 = DIRECTION('ref_axis',(0.924127230956645,0.0231154232803138,0.381385026201837)) ;
#17437 = DIRECTION('',(0.382084887170905,-0.0559079744467155,-0.922434516585791)) ;
#17438 = DIRECTION('center_axis',(0.705811580947719,-0.0604981355097965,-0.70581158094772)) ;
#17439 = DIRECTION('ref_axis',(0.707106781186549,1.90609208557029E-14,0.707106781186546)) ;
#17440 = DIRECTION('center_axis',(-0.922434516585792,0.0559079744467155,0.382084887170904)) ;
#17441 = DIRECTION('ref_axis',(0.386153547971707,0.133551654912738,0.912715395322623)) ;
#17442 = DIRECTION('',(0.922434516585791,-0.0559079744467155,-0.382084887170904)) ;
#17443 = DIRECTION('center_axis',(0.99816831025626,-0.0604981355098033,-3.28335275692119E-14)) ;
#17444 = DIRECTION('ref_axis',(3.28937148703078E-14,4.16807352605788E-16,
1.)) ;
#17445 = DIRECTION('center_axis',(0.99816831025626,-0.0604981355098033,-3.28335275692119E-14)) ;
#17446 = DIRECTION('ref_axis',(3.28937148703078E-14,4.16807352605788E-16,
1.)) ;
#17447 = DIRECTION('center_axis',(-0.922434516585791,0.0559079744467157,-0.382084887170905)) ;
#17448 = DIRECTION('ref_axis',(0.386153547971708,0.133551654912738,-0.912715395322622)) ;
#17449 = DIRECTION('',(0.922434516585791,-0.0559079744467157,0.382084887170906)) ;
#17450 = DIRECTION('center_axis',(0.70581158094776,-0.0604981355097965,0.705811580947679)) ;
#17451 = DIRECTION('ref_axis',(0.707106781186506,-1.64959525319754E-14,-0.707106781186589)) ;
#17452 = DIRECTION('center_axis',(0.70581158094776,-0.0604981355097965,0.705811580947679)) ;
#17453 = DIRECTION('ref_axis',(0.707106781186506,-1.64959525319754E-14,-0.707106781186589)) ;
#17454 = DIRECTION('center_axis',(0.70581158094776,-0.0604981355097965,0.705811580947679)) ;
#17455 = DIRECTION('ref_axis',(0.707106781186506,-1.64959525319754E-14,-0.707106781186589)) ;
#17456 = DIRECTION('center_axis',(-0.382084887170906,0.0559079744467155,-0.922434516585791)) ;
#17457 = DIRECTION('ref_axis',(0.924127230956645,0.0231154232803138,-0.381385026201837)) ;
#17458 = DIRECTION('',(0.382084887170905,-0.0559079744467155,0.922434516585791)) ;
#17459 = DIRECTION('center_axis',(0.382084887170906,-0.0559079744467155,0.922434516585791)) ;
#17460 = DIRECTION('ref_axis',(0.924127230956645,0.0231154232803138,-0.381385026201837)) ;
#17461 = DIRECTION('center_axis',(0.382084887170906,-0.0559079744467155,0.922434516585791)) ;
#17462 = DIRECTION('ref_axis',(-0.924127230956645,-0.0231154232803138,0.381385026201837)) ;
#17463 = DIRECTION('axis',(0.,0.,1.)) ;
#17464 = DIRECTION('refdir',(1.,0.,0.)) ;
#17465 = DIRECTION('center_axis',(0.,0.,1.)) ;
#17466 = DIRECTION('ref_axis',(1.,0.,0.)) ;
#17467 = DIRECTION('center_axis',(-0.350791170819065,0.,-0.936453711870154)) ;
#17468 = DIRECTION('ref_axis',(0.,-1.,0.)) ;
#17469 = DIRECTION('center_axis',(0.,1.,0.)) ;
#17470 = DIRECTION('ref_axis',(-1.,0.,0.)) ;
#17471 = DIRECTION('center_axis',(0.,0.,1.)) ;
#17472 = DIRECTION('ref_axis',(1.,0.,0.)) ;
#17473 = DIRECTION('center_axis',(0.,-1.,0.)) ;
#17474 = DIRECTION('ref_axis',(-1.,0.,0.)) ;
#17475 = DIRECTION('center_axis',(0.,0.,1.)) ;
#17476 = DIRECTION('ref_axis',(1.,0.,0.)) ;
#17477 = DIRECTION('center_axis',(0.350791170819065,0.,0.936453711870154)) ;
#17478 = DIRECTION('ref_axis',(0.,1.,0.)) ;
#17479 = DIRECTION('center_axis',(0.,1.,0.)) ;
#17480 = DIRECTION('ref_axis',(-1.,0.,0.)) ;
#17481 = DIRECTION('center_axis',(0.,0.,1.)) ;
#17482 = DIRECTION('ref_axis',(1.,0.,0.)) ;
#17483 = DIRECTION('center_axis',(0.,1.,0.)) ;
#17484 = DIRECTION('ref_axis',(-1.,0.,0.)) ;
#17485 = DIRECTION('center_axis',(0.,0.,1.)) ;
#17486 = DIRECTION('ref_axis',(1.,0.,0.)) ;
#17487 = DIRECTION('center_axis',(-0.350791170819065,0.,-0.936453711870154)) ;
#17488 = DIRECTION('ref_axis',(0.,-1.,0.)) ;
#17489 = DIRECTION('center_axis',(0.,1.,0.)) ;
#17490 = DIRECTION('ref_axis',(1.,0.,0.)) ;
#17491 = DIRECTION('center_axis',(0.,1.,0.)) ;
#17492 = DIRECTION('ref_axis',(1.,0.,0.)) ;
#17493 = DIRECTION('center_axis',(0.,0.,1.)) ;
#17494 = DIRECTION('ref_axis',(1.,0.,0.)) ;
#17495 = DIRECTION('center_axis',(0.,0.,1.)) ;
#17496 = DIRECTION('ref_axis',(1.,0.,0.)) ;
#17497 = DIRECTION('center_axis',(-0.201200039678648,0.,-0.979550174331724)) ;
#17498 = DIRECTION('ref_axis',(0.,-1.,0.)) ;
#17499 = DIRECTION('center_axis',(0.,-1.,0.)) ;
#17500 = DIRECTION('ref_axis',(-1.,0.,0.)) ;
#17501 = DIRECTION('center_axis',(0.,0.,1.)) ;
#17502 = DIRECTION('ref_axis',(1.,0.,0.)) ;
#17503 = DIRECTION('center_axis',(0.,1.,0.)) ;
#17504 = DIRECTION('ref_axis',(-1.,0.,0.)) ;
#17505 = DIRECTION('center_axis',(-0.350791170819065,0.,-0.936453711870154)) ;
#17506 = DIRECTION('ref_axis',(0.,-1.,0.)) ;
#17507 = DIRECTION('center_axis',(1.,0.,0.)) ;
#17508 = DIRECTION('ref_axis',(0.,-1.,0.)) ;
#17509 = DIRECTION('center_axis',(0.,1.,0.)) ;
#17510 = DIRECTION('ref_axis',(1.,0.,0.)) ;
#17511 = DIRECTION('center_axis',(0.,1.,0.)) ;
#17512 = DIRECTION('ref_axis',(1.,0.,0.)) ;
#17513 = DIRECTION('center_axis',(0.,0.,1.)) ;
#17514 = DIRECTION('ref_axis',(1.,0.,0.)) ;
#17515 = DIRECTION('center_axis',(-0.0467328634842026,0.,-0.998907422872894)) ;
#17516 = DIRECTION('ref_axis',(0.,-1.,0.)) ;
#17517 = DIRECTION('center_axis',(0.,1.,0.)) ;
#17518 = DIRECTION('ref_axis',(-1.,0.,0.)) ;
#17519 = DIRECTION('center_axis',(-0.201200039678648,0.,-0.979550174331724)) ;
#17520 = DIRECTION('ref_axis',(0.,-1.,0.)) ;
#17521 = DIRECTION('center_axis',(0.,0.,1.)) ;
#17522 = DIRECTION('ref_axis',(1.,0.,0.)) ;
#17523 = DIRECTION('center_axis',(0.,-1.,0.)) ;
#17524 = DIRECTION('ref_axis',(-1.,0.,0.)) ;
#17525 = DIRECTION('center_axis',(0.,0.,1.)) ;
#17526 = DIRECTION('ref_axis',(1.,0.,0.)) ;
#17527 = DIRECTION('center_axis',(0.,-1.,0.)) ;
#17528 = DIRECTION('ref_axis',(-1.,0.,0.)) ;
#17529 = DIRECTION('center_axis',(0.,0.,1.)) ;
#17530 = DIRECTION('ref_axis',(1.,0.,0.)) ;
#17531 = DIRECTION('center_axis',(0.0467328634842026,0.,0.998907422872894)) ;
#17532 = DIRECTION('ref_axis',(0.,1.,0.)) ;
#17533 = DIRECTION('center_axis',(0.,1.,0.)) ;
#17534 = DIRECTION('ref_axis',(-1.,0.,0.)) ;
#17535 = DIRECTION('center_axis',(0.,0.,1.)) ;
#17536 = DIRECTION('ref_axis',(1.,0.,0.)) ;
#17537 = DIRECTION('center_axis',(0.,1.,0.)) ;
#17538 = DIRECTION('ref_axis',(-1.,0.,0.)) ;
#17539 = DIRECTION('center_axis',(0.,0.,1.)) ;
#17540 = DIRECTION('ref_axis',(1.,0.,0.)) ;
#17541 = DIRECTION('center_axis',(0.108866874851964,0.,-0.99405633822232)) ;
#17542 = DIRECTION('ref_axis',(0.,-1.,0.)) ;
#17543 = DIRECTION('center_axis',(0.,-1.,0.)) ;
#17544 = DIRECTION('ref_axis',(-1.,0.,0.)) ;
#17545 = DIRECTION('center_axis',(0.,0.,1.)) ;
#17546 = DIRECTION('ref_axis',(1.,0.,0.)) ;
#17547 = DIRECTION('center_axis',(0.,1.,0.)) ;
#17548 = DIRECTION('ref_axis',(-1.,0.,0.)) ;
#17549 = DIRECTION('center_axis',(-0.0467328634842026,0.,-0.998907422872894)) ;
#17550 = DIRECTION('ref_axis',(0.,-1.,0.)) ;
#17551 = DIRECTION('center_axis',(0.,0.,1.)) ;
#17552 = DIRECTION('ref_axis',(1.,0.,0.)) ;
#17553 = DIRECTION('center_axis',(0.,-1.,0.)) ;
#17554 = DIRECTION('ref_axis',(-1.,0.,0.)) ;
#17555 = DIRECTION('center_axis',(0.,0.,1.)) ;
#17556 = DIRECTION('ref_axis',(1.,0.,0.)) ;
#17557 = DIRECTION('center_axis',(0.261828244987421,0.,-0.965114485502527)) ;
#17558 = DIRECTION('ref_axis',(0.,-1.,0.)) ;
#17559 = DIRECTION('center_axis',(0.,1.,0.)) ;
#17560 = DIRECTION('ref_axis',(-1.,0.,0.)) ;
#17561 = DIRECTION('center_axis',(0.108866874851964,0.,-0.99405633822232)) ;
#17562 = DIRECTION('ref_axis',(0.,-1.,0.)) ;
#17563 = DIRECTION('center_axis',(0.,0.,1.)) ;
#17564 = DIRECTION('ref_axis',(1.,0.,0.)) ;
#17565 = DIRECTION('center_axis',(0.,-1.,0.)) ;
#17566 = DIRECTION('ref_axis',(-1.,0.,0.)) ;
#17567 = DIRECTION('center_axis',(0.,0.,1.)) ;
#17568 = DIRECTION('ref_axis',(1.,0.,0.)) ;
#17569 = DIRECTION('center_axis',(0.,-1.,0.)) ;
#17570 = DIRECTION('ref_axis',(-1.,0.,0.)) ;
#17571 = DIRECTION('center_axis',(0.,0.,1.)) ;
#17572 = DIRECTION('ref_axis',(1.,0.,0.)) ;
#17573 = DIRECTION('center_axis',(-0.261828244987421,0.,0.965114485502527)) ;
#17574 = DIRECTION('ref_axis',(0.,1.,0.)) ;
#17575 = DIRECTION('center_axis',(0.,1.,0.)) ;
#17576 = DIRECTION('ref_axis',(-1.,0.,0.)) ;
#17577 = DIRECTION('center_axis',(0.,0.,1.)) ;
#17578 = DIRECTION('ref_axis',(1.,0.,0.)) ;
#17579 = DIRECTION('center_axis',(0.,1.,0.)) ;
#17580 = DIRECTION('ref_axis',(-1.,0.,0.)) ;
#17581 = DIRECTION('center_axis',(0.,0.,1.)) ;
#17582 = DIRECTION('ref_axis',(1.,0.,0.)) ;
#17583 = DIRECTION('center_axis',(0.408444256935997,0.,-0.912783265061319)) ;
#17584 = DIRECTION('ref_axis',(0.,-1.,0.)) ;
#17585 = DIRECTION('center_axis',(0.,-1.,0.)) ;
#17586 = DIRECTION('ref_axis',(-1.,0.,0.)) ;
#17587 = DIRECTION('center_axis',(0.,0.,1.)) ;
#17588 = DIRECTION('ref_axis',(1.,0.,0.)) ;
#17589 = DIRECTION('center_axis',(0.,1.,0.)) ;
#17590 = DIRECTION('ref_axis',(-1.,0.,0.)) ;
#17591 = DIRECTION('center_axis',(0.261828244987421,0.,-0.965114485502527)) ;
#17592 = DIRECTION('ref_axis',(0.,-1.,0.)) ;
#17593 = DIRECTION('center_axis',(0.,0.,1.)) ;
#17594 = DIRECTION('ref_axis',(1.,0.,0.)) ;
#17595 = DIRECTION('center_axis',(0.,-1.,0.)) ;
#17596 = DIRECTION('ref_axis',(-1.,0.,0.)) ;
#17597 = DIRECTION('center_axis',(0.,0.,1.)) ;
#17598 = DIRECTION('ref_axis',(1.,0.,0.)) ;
#17599 = DIRECTION('center_axis',(0.545161699271658,0.,-0.838330914166499)) ;
#17600 = DIRECTION('ref_axis',(0.,-1.,0.)) ;
#17601 = DIRECTION('center_axis',(0.,1.,0.)) ;
#17602 = DIRECTION('ref_axis',(-1.,0.,0.)) ;
#17603 = DIRECTION('center_axis',(0.408444256935997,0.,-0.912783265061319)) ;
#17604 = DIRECTION('ref_axis',(0.,-1.,0.)) ;
#17605 = DIRECTION('center_axis',(0.,0.,1.)) ;
#17606 = DIRECTION('ref_axis',(1.,0.,0.)) ;
#17607 = DIRECTION('center_axis',(0.,-1.,0.)) ;
#17608 = DIRECTION('ref_axis',(-1.,0.,0.)) ;
#17609 = DIRECTION('center_axis',(0.,0.,1.)) ;
#17610 = DIRECTION('ref_axis',(1.,0.,0.)) ;
#17611 = DIRECTION('center_axis',(0.,-1.,0.)) ;
#17612 = DIRECTION('ref_axis',(-1.,0.,0.)) ;
#17613 = DIRECTION('center_axis',(0.,0.,1.)) ;
#17614 = DIRECTION('ref_axis',(1.,0.,0.)) ;
#17615 = DIRECTION('center_axis',(-0.545161699271658,0.,0.838330914166499)) ;
#17616 = DIRECTION('ref_axis',(0.,1.,0.)) ;
#17617 = DIRECTION('center_axis',(0.,1.,0.)) ;
#17618 = DIRECTION('ref_axis',(-1.,0.,0.)) ;
#17619 = DIRECTION('center_axis',(0.,0.,1.)) ;
#17620 = DIRECTION('ref_axis',(1.,0.,0.)) ;
#17621 = DIRECTION('center_axis',(0.,1.,0.)) ;
#17622 = DIRECTION('ref_axis',(-1.,0.,0.)) ;
#17623 = DIRECTION('center_axis',(0.,0.,1.)) ;
#17624 = DIRECTION('ref_axis',(1.,0.,0.)) ;
#17625 = DIRECTION('center_axis',(0.668667250537987,0.,-0.743561771514626)) ;
#17626 = DIRECTION('ref_axis',(0.,-1.,0.)) ;
#17627 = DIRECTION('center_axis',(0.,-1.,0.)) ;
#17628 = DIRECTION('ref_axis',(-1.,0.,0.)) ;
#17629 = DIRECTION('center_axis',(0.,0.,1.)) ;
#17630 = DIRECTION('ref_axis',(1.,0.,0.)) ;
#17631 = DIRECTION('center_axis',(0.,1.,0.)) ;
#17632 = DIRECTION('ref_axis',(-1.,0.,0.)) ;
#17633 = DIRECTION('center_axis',(0.545161699271658,0.,-0.838330914166499)) ;
#17634 = DIRECTION('ref_axis',(0.,-1.,0.)) ;
#17635 = DIRECTION('center_axis',(0.,0.,1.)) ;
#17636 = DIRECTION('ref_axis',(1.,0.,0.)) ;
#17637 = DIRECTION('center_axis',(0.,-1.,0.)) ;
#17638 = DIRECTION('ref_axis',(-1.,0.,0.)) ;
#17639 = DIRECTION('center_axis',(0.,0.,1.)) ;
#17640 = DIRECTION('ref_axis',(1.,0.,0.)) ;
#17641 = DIRECTION('center_axis',(0.775967776969404,0.,-0.630772549422659)) ;
#17642 = DIRECTION('ref_axis',(0.,-1.,0.)) ;
#17643 = DIRECTION('center_axis',(0.,1.,0.)) ;
#17644 = DIRECTION('ref_axis',(-1.,0.,0.)) ;
#17645 = DIRECTION('center_axis',(0.668667250537987,0.,-0.743561771514626)) ;
#17646 = DIRECTION('ref_axis',(0.,-1.,0.)) ;
#17647 = DIRECTION('center_axis',(0.,0.,1.)) ;
#17648 = DIRECTION('ref_axis',(1.,0.,0.)) ;
#17649 = DIRECTION('center_axis',(0.,-1.,0.)) ;
#17650 = DIRECTION('ref_axis',(-1.,0.,0.)) ;
#17651 = DIRECTION('center_axis',(0.,0.,1.)) ;
#17652 = DIRECTION('ref_axis',(-0.999997170842168,0.00237871975216741,0.)) ;
#17653 = DIRECTION('center_axis',(0.,0.,1.)) ;
#17654 = DIRECTION('ref_axis',(1.,0.,0.)) ;
#17655 = DIRECTION('center_axis',(-0.775967776969404,0.,0.630772549422659)) ;
#17656 = DIRECTION('ref_axis',(0.,1.,0.)) ;
#17657 = DIRECTION('center_axis',(0.,0.,1.)) ;
#17658 = DIRECTION('ref_axis',(-0.999996539011801,-0.00263096264124049,0.)) ;
#17659 = DIRECTION('center_axis',(0.,0.,1.)) ;
#17660 = DIRECTION('ref_axis',(-0.999994323348501,-0.00336946149617212,0.)) ;
#17661 = DIRECTION('center_axis',(0.864462870524064,0.,-0.502696673437666)) ;
#17662 = DIRECTION('ref_axis',(0.,-1.,0.)) ;
#17663 = DIRECTION('center_axis',(0.,0.,1.)) ;
#17664 = DIRECTION('ref_axis',(1.,0.,0.)) ;
#17665 = DIRECTION('center_axis',(0.,1.,0.)) ;
#17666 = DIRECTION('ref_axis',(-1.,0.,0.)) ;
#17667 = DIRECTION('center_axis',(0.775967776969404,0.,-0.630772549422659)) ;
#17668 = DIRECTION('ref_axis',(0.,-1.,0.)) ;
#17669 = DIRECTION('center_axis',(0.,0.,1.)) ;
#17670 = DIRECTION('ref_axis',(1.,0.,0.)) ;
#17671 = DIRECTION('center_axis',(0.,0.,1.)) ;
#17672 = DIRECTION('ref_axis',(1.,0.,0.)) ;
#17673 = DIRECTION('center_axis',(0.864462870524064,0.,-0.502696673437666)) ;
#17674 = DIRECTION('ref_axis',(0.,-1.,0.)) ;
#17675 = DIRECTION('center_axis',(0.,1.,0.)) ;
#17676 = DIRECTION('ref_axis',(-1.,0.,0.)) ;
#17677 = DIRECTION('center_axis',(0.932007869282798,0.,-0.362438038283702)) ;
#17678 = DIRECTION('ref_axis',(0.362438038283702,0.,0.932007869282798)) ;
#17679 = DIRECTION('center_axis',(0.,0.,1.)) ;
#17680 = DIRECTION('ref_axis',(1.,0.,0.)) ;
#17681 = DIRECTION('center_axis',(0.,0.,1.)) ;
#17682 = DIRECTION('ref_axis',(-0.999991061612965,-0.00422808398397034,0.)) ;
#17683 = DIRECTION('center_axis',(0.,0.,1.)) ;
#17684 = DIRECTION('ref_axis',(1.,0.,0.)) ;
#17685 = DIRECTION('center_axis',(-0.932007869282798,0.,0.362438038283702)) ;
#17686 = DIRECTION('ref_axis',(-0.362438038283702,0.,-0.932007869282798)) ;
#17687 = DIRECTION('center_axis',(0.,0.,1.)) ;
#17688 = DIRECTION('ref_axis',(-0.99998657479322,0.00518172107739271,0.)) ;
#17689 = DIRECTION('center_axis',(0.,0.,1.)) ;
#17690 = DIRECTION('ref_axis',(-0.999999956889578,0.000293633856850915,0.)) ;
#17691 = DIRECTION('center_axis',(0.976965832926672,0.,-0.213395785557951)) ;
#17692 = DIRECTION('ref_axis',(0.213395785557951,0.,0.976965832926672)) ;
#17693 = DIRECTION('center_axis',(0.,0.,1.)) ;
#17694 = DIRECTION('ref_axis',(1.,0.,0.)) ;
#17695 = DIRECTION('center_axis',(0.932007869282798,0.,-0.362438038283702)) ;
#17696 = DIRECTION('ref_axis',(0.362438038283702,0.,0.932007869282798)) ;
#17697 = DIRECTION('center_axis',(0.,1.,0.)) ;
#17698 = DIRECTION('ref_axis',(-1.,0.,0.)) ;
#17699 = DIRECTION('center_axis',(0.932007869282798,0.,-0.362438038283702)) ;
#17700 = DIRECTION('ref_axis',(0.362438038283702,0.,0.932007869282798)) ;
#17701 = DIRECTION('center_axis',(0.,1.,0.)) ;
#17702 = DIRECTION('ref_axis',(-1.,0.,0.)) ;
#17703 = DIRECTION('center_axis',(0.,0.,1.)) ;
#17704 = DIRECTION('ref_axis',(1.,0.,0.)) ;
#17705 = DIRECTION('center_axis',(0.,0.,1.)) ;
#17706 = DIRECTION('ref_axis',(1.,0.,0.)) ;
#17707 = DIRECTION('center_axis',(0.976965832926672,0.,-0.213395785557951)) ;
#17708 = DIRECTION('ref_axis',(0.213395785557951,0.,0.976965832926672)) ;
#17709 = DIRECTION('center_axis',(0.,1.,0.)) ;
#17710 = DIRECTION('ref_axis',(-1.,0.,0.)) ;
#17711 = DIRECTION('center_axis',(0.976965832926672,0.,-0.213395785557951)) ;
#17712 = DIRECTION('ref_axis',(0.213395785557951,0.,0.976965832926672)) ;
#17713 = DIRECTION('center_axis',(0.,1.,0.)) ;
#17714 = DIRECTION('ref_axis',(-1.,0.,0.)) ;
#17715 = DIRECTION('center_axis',(0.998247213677188,0.,-0.0591819261745526)) ;
#17716 = DIRECTION('ref_axis',(0.0591819261745526,0.,0.998247213677188)) ;
#17717 = DIRECTION('center_axis',(0.,0.,1.)) ;
#17718 = DIRECTION('ref_axis',(1.,0.,0.)) ;
#17719 = DIRECTION('center_axis',(-5.94762334620619E-17,0.,1.)) ;
#17720 = DIRECTION('ref_axis',(-0.999999583069371,0.000913159944786785,0.)) ;
#17721 = DIRECTION('center_axis',(0.,0.,1.)) ;
#17722 = DIRECTION('ref_axis',(1.,0.,0.)) ;
#17723 = DIRECTION('center_axis',(-0.998247213677188,0.,0.0591819261745526)) ;
#17724 = DIRECTION('ref_axis',(-0.0591819261745526,0.,-0.998247213677188)) ;
#17725 = DIRECTION('center_axis',(-5.04646829375071E-17,0.,1.)) ;
#17726 = DIRECTION('ref_axis',(-0.999999999326038,3.67140843060554E-5,0.)) ;
#17727 = DIRECTION('center_axis',(0.,0.,1.)) ;
#17728 = DIRECTION('ref_axis',(1.,0.,0.)) ;
#17729 = DIRECTION('center_axis',(0.995336261281429,0.,0.0964661960393706)) ;
#17730 = DIRECTION('ref_axis',(-0.0964661960393706,0.,0.995336261281429)) ;
#17731 = DIRECTION('center_axis',(0.,1.,0.)) ;
#17732 = DIRECTION('ref_axis',(1.,0.,0.)) ;
#17733 = DIRECTION('center_axis',(0.,-1.,0.)) ;
#17734 = DIRECTION('ref_axis',(-0.995336261281429,0.,-0.0964661960393711)) ;
#17735 = DIRECTION('center_axis',(5.04646829375071E-17,0.,1.)) ;
#17736 = DIRECTION('ref_axis',(1.,0.,0.)) ;
#17737 = DIRECTION('center_axis',(0.,0.,1.)) ;
#17738 = DIRECTION('ref_axis',(-0.999999839691638,-0.000566230251627689,0.)) ;
#17739 = DIRECTION('center_axis',(-0.995336261281429,0.,-0.0964661960393706)) ;
#17740 = DIRECTION('ref_axis',(0.0964661960393706,0.,-0.995336261281429)) ;
#17741 = DIRECTION('center_axis',(5.04646829375071E-17,0.,1.)) ;
#17742 = DIRECTION('ref_axis',(1.,0.,0.)) ;
#17743 = DIRECTION('center_axis',(5.94762334620619E-17,0.,1.)) ;
#17744 = DIRECTION('ref_axis',(1.,0.,0.)) ;
#17745 = DIRECTION('center_axis',(0.995336261281429,0.,0.0964661960393706)) ;
#17746 = DIRECTION('ref_axis',(-0.0964661960393706,0.,0.995336261281429)) ;
#17747 = DIRECTION('center_axis',(0.995336261281429,0.,0.0964661960393706)) ;
#17748 = DIRECTION('ref_axis',(-0.0964661960393706,0.,0.995336261281429)) ;
#17749 = DIRECTION('center_axis',(0.,0.,1.)) ;
#17750 = DIRECTION('ref_axis',(1.,0.,0.)) ;
#17751 = DIRECTION('center_axis',(0.,1.,0.)) ;
#17752 = DIRECTION('ref_axis',(-1.,0.,0.)) ;
#17753 = DIRECTION('center_axis',(0.,1.,0.)) ;
#17754 = DIRECTION('ref_axis',(-1.,0.,0.)) ;
#17755 = DIRECTION('center_axis',(0.,0.,1.)) ;
#17756 = DIRECTION('ref_axis',(1.,0.,0.)) ;
#17757 = DIRECTION('center_axis',(0.995336261281429,0.,0.0964661960393706)) ;
#17758 = DIRECTION('ref_axis',(-0.0964661960393706,0.,0.995336261281429)) ;
#17759 = DIRECTION('center_axis',(0.,1.,0.)) ;
#17760 = DIRECTION('ref_axis',(1.,0.,0.)) ;
#17761 = DIRECTION('center_axis',(5.04646829375071E-17,0.,1.)) ;
#17762 = DIRECTION('ref_axis',(1.,0.,0.)) ;
#17763 = DIRECTION('center_axis',(0.998247213677188,0.,-0.0591819261745526)) ;
#17764 = DIRECTION('ref_axis',(0.0591819261745526,0.,0.998247213677188)) ;
#17765 = DIRECTION('center_axis',(0.,1.,0.)) ;
#17766 = DIRECTION('ref_axis',(-1.,0.,0.)) ;
#17767 = DIRECTION('center_axis',(0.998247213677188,0.,-0.0591819261745526)) ;
#17768 = DIRECTION('ref_axis',(0.0591819261745526,0.,0.998247213677188)) ;
#17769 = DIRECTION('center_axis',(0.,1.,0.)) ;
#17770 = DIRECTION('ref_axis',(-1.,0.,0.)) ;
#17771 = DIRECTION('center_axis',(0.,-1.,0.)) ;
#17772 = DIRECTION('ref_axis',(-0.995336261281429,0.,-0.0964661960393709)) ;
#17773 = DIRECTION('center_axis',(0.,0.,1.)) ;
#17774 = DIRECTION('ref_axis',(1.,0.,0.)) ;
#17775 = DIRECTION('center_axis',(0.,0.,1.)) ;
#17776 = DIRECTION('ref_axis',(-1.,0.,0.)) ;
#17777 = DIRECTION('center_axis',(-0.998247213677188,0.,0.0591819261745526)) ;
#17778 = DIRECTION('ref_axis',(0.0591819261745526,0.,0.998247213677188)) ;
#17779 = DIRECTION('center_axis',(-0.998247213677188,0.,0.0591819261745526)) ;
#17780 = DIRECTION('ref_axis',(0.0591819261745526,0.,0.998247213677188)) ;
#17781 = DIRECTION('center_axis',(0.976965832926672,0.,-0.213395785557951)) ;
#17782 = DIRECTION('ref_axis',(0.213395785557951,0.,0.976965832926672)) ;
#17783 = DIRECTION('center_axis',(0.976965832926672,0.,-0.213395785557951)) ;
#17784 = DIRECTION('ref_axis',(0.213395785557951,0.,0.976965832926672)) ;
#17785 = DIRECTION('center_axis',(0.,0.,1.)) ;
#17786 = DIRECTION('ref_axis',(-1.,0.,0.)) ;
#17787 = DIRECTION('center_axis',(-0.976965832926672,0.,0.213395785557951)) ;
#17788 = DIRECTION('ref_axis',(0.213395785557951,0.,0.976965832926672)) ;
#17789 = DIRECTION('center_axis',(-0.976965832926672,0.,0.213395785557951)) ;
#17790 = DIRECTION('ref_axis',(0.213395785557951,0.,0.976965832926672)) ;
#17791 = DIRECTION('center_axis',(0.932007869282798,0.,-0.362438038283702)) ;
#17792 = DIRECTION('ref_axis',(0.362438038283702,0.,0.932007869282798)) ;
#17793 = DIRECTION('center_axis',(0.932007869282798,0.,-0.362438038283702)) ;
#17794 = DIRECTION('ref_axis',(0.362438038283702,0.,0.932007869282798)) ;
#17795 = DIRECTION('center_axis',(0.,0.,1.)) ;
#17796 = DIRECTION('ref_axis',(-1.,-6.34413156928661E-16,0.)) ;
#17797 = DIRECTION('center_axis',(-0.775967776969404,0.,0.630772549422659)) ;
#17798 = DIRECTION('ref_axis',(0.630772549422659,0.,0.775967776969404)) ;
#17799 = DIRECTION('center_axis',(-0.775967776969404,0.,0.630772549422659)) ;
#17800 = DIRECTION('ref_axis',(0.630772549422659,0.,0.775967776969404)) ;
#17801 = DIRECTION('center_axis',(0.668667250537987,0.,-0.743561771514626)) ;
#17802 = DIRECTION('ref_axis',(0.743561771514626,0.,0.668667250537987)) ;
#17803 = DIRECTION('center_axis',(0.668667250537987,0.,-0.743561771514626)) ;
#17804 = DIRECTION('ref_axis',(0.743561771514626,0.,0.668667250537987)) ;
#17805 = DIRECTION('center_axis',(0.,0.,1.)) ;
#17806 = DIRECTION('ref_axis',(-1.,0.,0.)) ;
#17807 = DIRECTION('center_axis',(-0.668667250537987,0.,0.743561771514626)) ;
#17808 = DIRECTION('ref_axis',(0.743561771514626,0.,0.668667250537987)) ;
#17809 = DIRECTION('center_axis',(-0.668667250537987,0.,0.743561771514626)) ;
#17810 = DIRECTION('ref_axis',(0.743561771514626,0.,0.668667250537987)) ;
#17811 = DIRECTION('center_axis',(0.545161699271658,0.,-0.838330914166499)) ;
#17812 = DIRECTION('ref_axis',(0.838330914166499,0.,0.545161699271658)) ;
#17813 = DIRECTION('center_axis',(0.545161699271658,0.,-0.838330914166499)) ;
#17814 = DIRECTION('ref_axis',(0.838330914166499,0.,0.545161699271658)) ;
#17815 = DIRECTION('center_axis',(0.,0.,1.)) ;
#17816 = DIRECTION('ref_axis',(-1.,0.,0.)) ;
#17817 = DIRECTION('center_axis',(-0.261828244987421,0.,0.965114485502527)) ;
#17818 = DIRECTION('ref_axis',(0.965114485502527,0.,0.261828244987421)) ;
#17819 = DIRECTION('center_axis',(-0.261828244987421,0.,0.965114485502527)) ;
#17820 = DIRECTION('ref_axis',(0.965114485502527,0.,0.261828244987421)) ;
#17821 = DIRECTION('center_axis',(0.108866874851964,0.,-0.99405633822232)) ;
#17822 = DIRECTION('ref_axis',(0.99405633822232,0.,0.108866874851965)) ;
#17823 = DIRECTION('center_axis',(0.108866874851964,0.,-0.99405633822232)) ;
#17824 = DIRECTION('ref_axis',(0.99405633822232,0.,0.108866874851965)) ;
#17825 = DIRECTION('center_axis',(0.,0.,1.)) ;
#17826 = DIRECTION('ref_axis',(-1.,0.,0.)) ;
#17827 = DIRECTION('center_axis',(-0.108866874851964,0.,0.99405633822232)) ;
#17828 = DIRECTION('ref_axis',(0.99405633822232,0.,0.108866874851965)) ;
#17829 = DIRECTION('center_axis',(-0.108866874851964,0.,0.99405633822232)) ;
#17830 = DIRECTION('ref_axis',(0.99405633822232,0.,0.108866874851965)) ;
#17831 = DIRECTION('center_axis',(-0.0467328634842026,0.,-0.998907422872894)) ;
#17832 = DIRECTION('ref_axis',(0.998907422872894,0.,-0.0467328634842026)) ;
#17833 = DIRECTION('center_axis',(-0.0467328634842026,0.,-0.998907422872894)) ;
#17834 = DIRECTION('ref_axis',(0.998907422872894,0.,-0.0467328634842026)) ;
#17835 = DIRECTION('center_axis',(0.,0.,1.)) ;
#17836 = DIRECTION('ref_axis',(1.,0.,0.)) ;
#17837 = DIRECTION('center_axis',(0.350791170819065,0.,0.936453711870154)) ;
#17838 = DIRECTION('ref_axis',(0.936453711870154,0.,-0.350791170819065)) ;
#17839 = DIRECTION('center_axis',(0.,1.,0.)) ;
#17840 = DIRECTION('ref_axis',(1.,0.,0.)) ;
#17841 = DIRECTION('center_axis',(0.577350269189626,0.577350269189626,0.577350269189626)) ;
#17842 = DIRECTION('ref_axis',(-0.707106781186548,0.,0.707106781186548)) ;
#17843 = DIRECTION('center_axis',(0.350791170819065,0.,0.936453711870154)) ;
#17844 = DIRECTION('ref_axis',(0.936453711870154,0.,-0.350791170819065)) ;
#17845 = DIRECTION('center_axis',(-0.408248290463863,0.816496580927726,-0.408248290463863)) ;
#17846 = DIRECTION('ref_axis',(0.707106781186548,0.,-0.707106781186548)) ;
#17847 = DIRECTION('center_axis',(0.350791170819065,0.,0.936453711870154)) ;
#17848 = DIRECTION('ref_axis',(0.936453711870154,0.,-0.350791170819065)) ;
#17849 = DIRECTION('center_axis',(0.,1.,0.)) ;
#17850 = DIRECTION('ref_axis',(1.,0.,0.)) ;
#17851 = DIRECTION('center_axis',(0.,1.,0.)) ;
#17852 = DIRECTION('ref_axis',(1.,0.,0.)) ;
#17853 = DIRECTION('center_axis',(0.,1.,0.)) ;
#17854 = DIRECTION('ref_axis',(1.,0.,0.)) ;
#17855 = DIRECTION('',(0.,1.,0.)) ;
#17856 = DIRECTION('center_axis',(0.,-1.,0.)) ;
#17857 = DIRECTION('ref_axis',(1.,0.,0.)) ;
#17858 = DIRECTION('center_axis',(0.,-1.,0.)) ;
#17859 = DIRECTION('ref_axis',(1.,0.,0.)) ;
#17860 = DIRECTION('',(0.,1.,0.)) ;
#17861 = DIRECTION('center_axis',(-0.703809019912964,0.707106781186547,-0.0682119013747098)) ;
#17862 = DIRECTION('ref_axis',(0.703809019912964,0.707106781186548,0.0682119013747098)) ;
#17863 = DIRECTION('center_axis',(0.,1.,0.)) ;
#17864 = DIRECTION('ref_axis',(1.,0.,0.)) ;
#17865 = DIRECTION('center_axis',(0.,1.,0.)) ;
#17866 = DIRECTION('ref_axis',(1.,0.,0.)) ;
#17867 = DIRECTION('center_axis',(-0.703809019912964,0.707106781186547,-0.0682119013747098)) ;
#17868 = DIRECTION('ref_axis',(0.703809019912964,0.707106781186548,0.0682119013747098)) ;
#17869 = DIRECTION('center_axis',(0.,-1.,0.)) ;
#17870 = DIRECTION('ref_axis',(1.,0.,0.)) ;
#17871 = DIRECTION('center_axis',(0.,1.,0.)) ;
#17872 = DIRECTION('ref_axis',(1.,0.,0.)) ;
#17873 = DIRECTION('center_axis',(0.995336261281429,0.,0.0964661960393706)) ;
#17874 = DIRECTION('ref_axis',(0.0964661960393706,0.,-0.995336261281429)) ;
#17875 = DIRECTION('',(-0.995336261281429,0.,-0.0964661960393706)) ;
#17876 = DIRECTION('center_axis',(-0.999825160912746,0.,-0.0186988664309099)) ;
#17877 = DIRECTION('ref_axis',(0.0186988664309099,0.,-0.999825160912746)) ;
#17878 = DIRECTION('center_axis',(-0.995336261281429,0.,-0.0964661960393706)) ;
#17879 = DIRECTION('ref_axis',(0.0964661960393706,0.,-0.995336261281429)) ;
#17880 = DIRECTION('center_axis',(-0.999825160912746,0.,-0.0186988664309099)) ;
#17881 = DIRECTION('ref_axis',(0.0186988664309099,0.,-0.999825160912746)) ;
#17882 = DIRECTION('center_axis',(0.995336261281429,0.,0.0964661960393706)) ;
#17883 = DIRECTION('ref_axis',(0.0964661960393706,0.,-0.995336261281429)) ;
#17884 = DIRECTION('center_axis',(0.995336261281429,0.,0.0964661960393706)) ;
#17885 = DIRECTION('ref_axis',(0.0964661960393706,0.,-0.995336261281429)) ;
#17886 = DIRECTION('center_axis',(0.995336261281429,0.,0.0964661960393706)) ;
#17887 = DIRECTION('ref_axis',(0.0964661960393706,0.,-0.995336261281429)) ;
#17888 = DIRECTION('center_axis',(0.998247213677188,0.,-0.0591819261745526)) ;
#17889 = DIRECTION('ref_axis',(0.0591819261745526,0.,0.998247213677188)) ;
#17890 = DIRECTION('center_axis',(0.998247213677188,0.,-0.0591819261745526)) ;
#17891 = DIRECTION('ref_axis',(0.0591819261745526,0.,0.998247213677188)) ;
#17892 = DIRECTION('',(-0.998247213677188,0.,0.0591819261745526)) ;
#17893 = DIRECTION('center_axis',(-0.990611994413054,0.,0.136703608310067)) ;
#17894 = DIRECTION('ref_axis',(0.136703608310067,0.,0.990611994413054)) ;
#17895 = DIRECTION('center_axis',(0.998247213677188,0.,-0.0591819261745526)) ;
#17896 = DIRECTION('ref_axis',(0.0591819261745526,0.,0.998247213677188)) ;
#17897 = DIRECTION('center_axis',(0.976965832926672,0.,-0.213395785557951)) ;
#17898 = DIRECTION('ref_axis',(0.213395785557951,0.,0.976965832926672)) ;
#17899 = DIRECTION('',(-0.976965832926672,0.,0.213395785557951)) ;
#17900 = DIRECTION('center_axis',(-0.957391532867416,0.,0.288793096859637)) ;
#17901 = DIRECTION('ref_axis',(0.288793096859637,0.,0.957391532867416)) ;
#17902 = DIRECTION('center_axis',(0.932007869282798,0.,-0.362438038283702)) ;
#17903 = DIRECTION('ref_axis',(0.362438038283702,0.,0.932007869282798)) ;
#17904 = DIRECTION('',(-0.932007869282798,0.,0.362438038283702)) ;
#17905 = DIRECTION('center_axis',(-0.932007869282798,0.,0.362438038283702)) ;
#17906 = DIRECTION('ref_axis',(0.362438038283702,0.,0.932007869282798)) ;
#17907 = DIRECTION('center_axis',(-0.900968867902422,0.,0.433883739117552)) ;
#17908 = DIRECTION('ref_axis',(0.433883739117552,0.,0.900968867902422)) ;
#17909 = DIRECTION('center_axis',(-0.932007869282798,0.,0.362438038283702)) ;
#17910 = DIRECTION('ref_axis',(0.362438038283702,0.,0.932007869282798)) ;
#17911 = DIRECTION('center_axis',(0.864462870524064,0.,-0.502696673437666)) ;
#17912 = DIRECTION('ref_axis',(0.502696673437666,0.,0.864462870524064)) ;
#17913 = DIRECTION('center_axis',(0.864462870524064,0.,-0.502696673437666)) ;
#17914 = DIRECTION('ref_axis',(0.502696673437666,0.,0.864462870524064)) ;
#17915 = DIRECTION('',(-0.864462870524064,0.,0.502696673437666)) ;
#17916 = DIRECTION('center_axis',(-0.864462870524064,0.,0.502696673437666)) ;
#17917 = DIRECTION('ref_axis',(0.502696673437666,0.,0.864462870524064)) ;
#17918 = DIRECTION('center_axis',(-0.822711392173034,0.,0.568459290704891)) ;
#17919 = DIRECTION('ref_axis',(0.568459290704891,0.,0.822711392173034)) ;
#17920 = DIRECTION('center_axis',(-0.864462870524064,0.,0.502696673437666)) ;
#17921 = DIRECTION('ref_axis',(0.502696673437666,0.,0.864462870524064)) ;
#17922 = DIRECTION('center_axis',(0.864462870524064,0.,-0.502696673437666)) ;
#17923 = DIRECTION('ref_axis',(0.502696673437666,0.,0.864462870524064)) ;
#17924 = DIRECTION('center_axis',(0.775967776969404,0.,-0.630772549422659)) ;
#17925 = DIRECTION('ref_axis',(0.630772549422659,0.,0.775967776969404)) ;
#17926 = DIRECTION('center_axis',(0.775967776969404,0.,-0.630772549422659)) ;
#17927 = DIRECTION('ref_axis',(0.630772549422659,0.,0.775967776969404)) ;
#17928 = DIRECTION('',(-0.775967776969404,0.,0.630772549422659)) ;
#17929 = DIRECTION('center_axis',(-0.724515660859275,0.,0.689258338483945)) ;
#17930 = DIRECTION('ref_axis',(0.689258338483945,0.,0.724515660859275)) ;
#17931 = DIRECTION('center_axis',(0.775967776969404,0.,-0.630772549422659)) ;
#17932 = DIRECTION('ref_axis',(0.630772549422659,0.,0.775967776969404)) ;
#17933 = DIRECTION('center_axis',(0.668667250537987,0.,-0.743561771514626)) ;
#17934 = DIRECTION('ref_axis',(0.743561771514626,0.,0.668667250537987)) ;
#17935 = DIRECTION('',(-0.668667250537987,0.,0.743561771514626)) ;
#17936 = DIRECTION('center_axis',(-0.608761429008721,0.,0.793353340291235)) ;
#17937 = DIRECTION('ref_axis',(0.793353340291235,0.,0.608761429008721)) ;
#17938 = DIRECTION('center_axis',(0.545161699271658,0.,-0.838330914166499)) ;
#17939 = DIRECTION('ref_axis',(0.838330914166499,0.,0.545161699271658)) ;
#17940 = DIRECTION('',(-0.545161699271658,0.,0.838330914166499)) ;
#17941 = DIRECTION('center_axis',(-0.545161699271658,0.,0.838330914166499)) ;
#17942 = DIRECTION('ref_axis',(0.838330914166499,0.,0.545161699271658)) ;
#17943 = DIRECTION('center_axis',(-0.478253978621312,0.,0.878221573370232)) ;
#17944 = DIRECTION('ref_axis',(0.878221573370232,0.,0.478253978621312)) ;
#17945 = DIRECTION('center_axis',(-0.545161699271658,0.,0.838330914166499)) ;
#17946 = DIRECTION('ref_axis',(0.838330914166499,0.,0.545161699271658)) ;
#17947 = DIRECTION('center_axis',(0.408444256935997,0.,-0.912783265061319)) ;
#17948 = DIRECTION('ref_axis',(0.912783265061319,0.,0.408444256935996)) ;
#17949 = DIRECTION('center_axis',(0.408444256935997,0.,-0.912783265061319)) ;
#17950 = DIRECTION('ref_axis',(0.912783265061319,0.,0.408444256935996)) ;
#17951 = DIRECTION('',(-0.408444256935996,0.,0.912783265061319)) ;
#17952 = DIRECTION('center_axis',(-0.408444256935997,0.,0.912783265061319)) ;
#17953 = DIRECTION('ref_axis',(0.912783265061319,0.,0.408444256935996)) ;
#17954 = DIRECTION('center_axis',(-0.336156133168625,0.,0.941806272082066)) ;
#17955 = DIRECTION('ref_axis',(0.941806272082065,0.,0.336156133168625)) ;
#17956 = DIRECTION('center_axis',(-0.408444256935997,0.,0.912783265061319)) ;
#17957 = DIRECTION('ref_axis',(0.912783265061319,0.,0.408444256935996)) ;
#17958 = DIRECTION('center_axis',(0.408444256935997,0.,-0.912783265061319)) ;
#17959 = DIRECTION('ref_axis',(0.912783265061319,0.,0.408444256935996)) ;
#17960 = DIRECTION('center_axis',(0.261828244987421,0.,-0.965114485502527)) ;
#17961 = DIRECTION('ref_axis',(0.965114485502527,0.,0.261828244987421)) ;
#17962 = DIRECTION('center_axis',(0.261828244987421,0.,-0.965114485502527)) ;
#17963 = DIRECTION('ref_axis',(0.965114485502527,0.,0.261828244987421)) ;
#17964 = DIRECTION('',(-0.261828244987421,0.,0.965114485502527)) ;
#17965 = DIRECTION('center_axis',(-0.185911607162916,0.,0.982566473233288)) ;
#17966 = DIRECTION('ref_axis',(0.982566473233288,0.,0.185911607162916)) ;
#17967 = DIRECTION('center_axis',(0.261828244987421,0.,-0.965114485502527)) ;
#17968 = DIRECTION('ref_axis',(0.965114485502527,0.,0.261828244987421)) ;
#17969 = DIRECTION('center_axis',(0.108866874851964,0.,-0.99405633822232)) ;
#17970 = DIRECTION('ref_axis',(0.99405633822232,0.,0.108866874851965)) ;
#17971 = DIRECTION('',(-0.108866874851965,0.,0.99405633822232)) ;
#17972 = DIRECTION('center_axis',(-0.0311615483847374,0.,0.999514361028528)) ;
#17973 = DIRECTION('ref_axis',(0.999514361028528,0.,0.0311615483847374)) ;
#17974 = DIRECTION('center_axis',(-0.0467328634842026,0.,-0.998907422872894)) ;
#17975 = DIRECTION('ref_axis',(0.998907422872894,0.,-0.0467328634842026)) ;
#17976 = DIRECTION('',(0.0467328634842026,0.,0.998907422872894)) ;
#17977 = DIRECTION('center_axis',(0.0467328634842026,0.,0.998907422872894)) ;
#17978 = DIRECTION('ref_axis',(0.998907422872894,0.,-0.0467328634842026)) ;
#17979 = DIRECTION('center_axis',(0.124343704647499,0.,0.99223920660017)) ;
#17980 = DIRECTION('ref_axis',(0.99223920660017,0.,-0.124343704647499)) ;
#17981 = DIRECTION('center_axis',(0.0467328634842026,0.,0.998907422872894)) ;
#17982 = DIRECTION('ref_axis',(0.998907422872894,0.,-0.0467328634842026)) ;
#17983 = DIRECTION('center_axis',(-0.201200039678648,0.,-0.979550174331724)) ;
#17984 = DIRECTION('ref_axis',(0.979550174331724,0.,-0.201200039678648)) ;
#17985 = DIRECTION('center_axis',(-0.201200039678648,0.,-0.979550174331724)) ;
#17986 = DIRECTION('ref_axis',(0.979550174331724,0.,-0.201200039678648)) ;
#17987 = DIRECTION('',(0.201200039678648,0.,0.979550174331724)) ;
#17988 = DIRECTION('center_axis',(0.201200039678648,0.,0.979550174331724)) ;
#17989 = DIRECTION('ref_axis',(0.979550174331724,0.,-0.201200039678648)) ;
#17990 = DIRECTION('center_axis',(0.276835511424842,0.,0.960917321945102)) ;
#17991 = DIRECTION('ref_axis',(0.960917321945102,0.,-0.276835511424842)) ;
#17992 = DIRECTION('center_axis',(0.201200039678648,0.,0.979550174331724)) ;
#17993 = DIRECTION('ref_axis',(0.979550174331724,0.,-0.201200039678648)) ;
#17994 = DIRECTION('center_axis',(-0.201200039678648,0.,-0.979550174331724)) ;
#17995 = DIRECTION('ref_axis',(0.979550174331724,0.,-0.201200039678648)) ;
#17996 = DIRECTION('center_axis',(-0.350791170819065,0.,-0.936453711870154)) ;
#17997 = DIRECTION('ref_axis',(0.936453711870154,0.,-0.350791170819065)) ;
#17998 = DIRECTION('center_axis',(-0.350791170819065,0.,-0.936453711870154)) ;
#17999 = DIRECTION('ref_axis',(0.936453711870154,0.,-0.350791170819065)) ;
#18000 = DIRECTION('',(0.350791170819065,0.,0.936453711870154)) ;
#18001 = DIRECTION('center_axis',(0.248046815666529,-0.707106781186547,0.6621727699307)) ;
#18002 = DIRECTION('ref_axis',(-0.248046815666529,-0.707106781186548,-0.662172769930699)) ;
#18003 = DIRECTION('center_axis',(0.248046815666529,-0.707106781186547,0.6621727699307)) ;
#18004 = DIRECTION('ref_axis',(-0.248046815666529,-0.707106781186548,-0.662172769930699)) ;
#18005 = DIRECTION('center_axis',(-0.350791170819065,0.,-0.936453711870154)) ;
#18006 = DIRECTION('ref_axis',(0.936453711870154,0.,-0.350791170819065)) ;
#18007 = DIRECTION('center_axis',(-0.350791170819065,0.,-0.936453711870154)) ;
#18008 = DIRECTION('ref_axis',(0.936453711870154,0.,-0.350791170819065)) ;
#18009 = DIRECTION('center_axis',(0.,1.,0.)) ;
#18010 = DIRECTION('ref_axis',(1.,0.,0.)) ;
#18011 = DIRECTION('',(0.,-1.,0.)) ;
#18012 = DIRECTION('center_axis',(0.,-1.,0.)) ;
#18013 = DIRECTION('ref_axis',(1.,0.,0.)) ;
#18014 = DIRECTION('center_axis',(0.,-1.,0.)) ;
#18015 = DIRECTION('ref_axis',(-1.,0.,0.)) ;
#18016 = DIRECTION('center_axis',(0.,0.,1.)) ;
#18017 = DIRECTION('ref_axis',(-1.,0.,0.)) ;
#18018 = DIRECTION('center_axis',(0.,0.,1.)) ;
#18019 = DIRECTION('ref_axis',(-1.,0.,0.)) ;
#18020 = DIRECTION('center_axis',(0.,0.,1.)) ;
#18021 = DIRECTION('ref_axis',(-1.,0.,0.)) ;
#18022 = DIRECTION('center_axis',(0.,0.,1.)) ;
#18023 = DIRECTION('ref_axis',(-1.,0.,0.)) ;
#18024 = DIRECTION('center_axis',(0.,0.,1.)) ;
#18025 = DIRECTION('ref_axis',(-1.,0.,0.)) ;
#18026 = DIRECTION('center_axis',(0.,0.,1.)) ;
#18027 = DIRECTION('ref_axis',(-1.,0.,0.)) ;
#18028 = DIRECTION('center_axis',(5.94762334620619E-17,0.,1.)) ;
#18029 = DIRECTION('ref_axis',(1.,0.,0.)) ;
#18030 = DIRECTION('center_axis',(0.,-1.,0.)) ;
#18031 = DIRECTION('ref_axis',(-1.,0.,0.)) ;
#18032 = DIRECTION('center_axis',(0.,-1.,0.)) ;
#18033 = DIRECTION('ref_axis',(1.,0.,0.)) ;
#18034 = DIRECTION('center_axis',(0.,1.,0.)) ;
#18035 = DIRECTION('ref_axis',(1.,0.,0.)) ;
#18036 = DIRECTION('',(0.,-1.,0.)) ;
#18037 = DIRECTION('center_axis',(0.577350269189626,0.577350269189626,0.577350269189626)) ;
#18038 = DIRECTION('ref_axis',(-0.707106781186548,0.,0.707106781186547)) ;
#18039 = DIRECTION('center_axis',(-0.408248290463863,0.816496580927726,-0.408248290463863)) ;
#18040 = DIRECTION('ref_axis',(0.707106781186548,0.,-0.707106781186547)) ;
#18041 = DIRECTION('center_axis',(0.,0.,1.)) ;
#18042 = DIRECTION('ref_axis',(1.,0.,0.)) ;
#18043 = DIRECTION('center_axis',(0.,0.,1.)) ;
#18044 = DIRECTION('ref_axis',(-0.999995485023846,-0.00300498451297073,0.)) ;
#18045 = DIRECTION('center_axis',(-0.976965832926672,0.,0.213395785557951)) ;
#18046 = DIRECTION('ref_axis',(-0.213395785557951,0.,-0.976965832926672)) ;
#18047 = DIRECTION('center_axis',(0.,0.,1.)) ;
#18048 = DIRECTION('ref_axis',(1.,0.,0.)) ;
#18049 = DIRECTION('center_axis',(0.,0.,1.)) ;
#18050 = DIRECTION('ref_axis',(-0.999998402547297,-0.00178742911851967,0.)) ;
#18051 = DIRECTION('center_axis',(-0.864462870524064,0.,0.502696673437666)) ;
#18052 = DIRECTION('ref_axis',(0.,1.,0.)) ;
#18053 = DIRECTION('center_axis',(0.,0.,1.)) ;
#18054 = DIRECTION('ref_axis',(1.,0.,0.)) ;
#18055 = DIRECTION('center_axis',(0.,0.,1.)) ;
#18056 = DIRECTION('ref_axis',(1.,0.,0.)) ;
#18057 = DIRECTION('center_axis',(-0.668667250537987,0.,0.743561771514626)) ;
#18058 = DIRECTION('ref_axis',(0.,1.,0.)) ;
#18059 = DIRECTION('center_axis',(0.,1.,0.)) ;
#18060 = DIRECTION('ref_axis',(-1.,0.,0.)) ;
#18061 = DIRECTION('center_axis',(0.,0.,1.)) ;
#18062 = DIRECTION('ref_axis',(1.,0.,0.)) ;
#18063 = DIRECTION('center_axis',(0.,1.,0.)) ;
#18064 = DIRECTION('ref_axis',(-1.,0.,0.)) ;
#18065 = DIRECTION('center_axis',(0.,0.,1.)) ;
#18066 = DIRECTION('ref_axis',(1.,0.,0.)) ;
#18067 = DIRECTION('center_axis',(-0.408444256935997,0.,0.912783265061319)) ;
#18068 = DIRECTION('ref_axis',(0.,1.,0.)) ;
#18069 = DIRECTION('center_axis',(0.,1.,0.)) ;
#18070 = DIRECTION('ref_axis',(-1.,0.,0.)) ;
#18071 = DIRECTION('center_axis',(0.,0.,1.)) ;
#18072 = DIRECTION('ref_axis',(1.,0.,0.)) ;
#18073 = DIRECTION('center_axis',(0.,1.,0.)) ;
#18074 = DIRECTION('ref_axis',(-1.,0.,0.)) ;
#18075 = DIRECTION('center_axis',(0.,0.,1.)) ;
#18076 = DIRECTION('ref_axis',(1.,0.,0.)) ;
#18077 = DIRECTION('center_axis',(-0.108866874851964,0.,0.99405633822232)) ;
#18078 = DIRECTION('ref_axis',(0.,1.,0.)) ;
#18079 = DIRECTION('center_axis',(0.,1.,0.)) ;
#18080 = DIRECTION('ref_axis',(-1.,0.,0.)) ;
#18081 = DIRECTION('center_axis',(0.,0.,1.)) ;
#18082 = DIRECTION('ref_axis',(1.,0.,0.)) ;
#18083 = DIRECTION('center_axis',(0.,1.,0.)) ;
#18084 = DIRECTION('ref_axis',(-1.,0.,0.)) ;
#18085 = DIRECTION('center_axis',(0.,0.,1.)) ;
#18086 = DIRECTION('ref_axis',(1.,0.,0.)) ;
#18087 = DIRECTION('center_axis',(0.201200039678648,0.,0.979550174331724)) ;
#18088 = DIRECTION('ref_axis',(0.,1.,0.)) ;
#18089 = DIRECTION('center_axis',(0.,1.,0.)) ;
#18090 = DIRECTION('ref_axis',(-1.,0.,0.)) ;
#18091 = DIRECTION('center_axis',(0.,0.,1.)) ;
#18092 = DIRECTION('ref_axis',(1.,0.,0.)) ;
#18093 = DIRECTION('center_axis',(0.,1.,0.)) ;
#18094 = DIRECTION('ref_axis',(-1.,0.,0.)) ;
#18095 = DIRECTION('axis',(0.,0.,1.)) ;
#18096 = DIRECTION('refdir',(1.,0.,0.)) ;
#18097 = DIRECTION('center_axis',(0.,0.,1.)) ;
#18098 = DIRECTION('ref_axis',(1.,0.,0.)) ;
#18099 = DIRECTION('center_axis',(0.,0.,1.)) ;
#18100 = DIRECTION('ref_axis',(1.,0.,0.)) ;
#18101 = DIRECTION('',(0.,0.,-1.)) ;
#18102 = DIRECTION('center_axis',(0.,0.,-1.)) ;
#18103 = DIRECTION('ref_axis',(1.,0.,0.)) ;
#18104 = DIRECTION('',(0.,0.,-1.)) ;
#18105 = DIRECTION('center_axis',(-1.,0.,0.)) ;
#18106 = DIRECTION('ref_axis',(0.,0.,1.)) ;
#18107 = DIRECTION('',(0.,1.,0.)) ;
#18108 = DIRECTION('',(0.,-1.,0.)) ;
#18109 = DIRECTION('',(0.,0.,-1.)) ;
#18110 = DIRECTION('center_axis',(0.,0.,1.)) ;
#18111 = DIRECTION('ref_axis',(1.,0.,0.)) ;
#18112 = DIRECTION('center_axis',(0.,0.,1.)) ;
#18113 = DIRECTION('ref_axis',(1.,0.,0.)) ;
#18114 = DIRECTION('center_axis',(0.,0.,-1.)) ;
#18115 = DIRECTION('ref_axis',(1.,0.,0.)) ;
#18116 = DIRECTION('',(0.,0.,-1.)) ;
#18117 = DIRECTION('center_axis',(1.,0.,0.)) ;
#18118 = DIRECTION('ref_axis',(0.,0.,-1.)) ;
#18119 = DIRECTION('',(0.,-1.,0.)) ;
#18120 = DIRECTION('',(0.,1.,0.)) ;
#18121 = DIRECTION('center_axis',(0.,1.,0.)) ;
#18122 = DIRECTION('ref_axis',(1.,0.,0.)) ;
#18123 = DIRECTION('center_axis',(0.,1.,0.)) ;
#18124 = DIRECTION('ref_axis',(1.,0.,0.)) ;
#18125 = DIRECTION('',(0.,1.,0.)) ;
#18126 = DIRECTION('center_axis',(0.,-1.,0.)) ;
#18127 = DIRECTION('ref_axis',(1.,0.,0.)) ;
#18128 = DIRECTION('center_axis',(0.,0.,1.)) ;
#18129 = DIRECTION('ref_axis',(1.,0.,0.)) ;
#18130 = DIRECTION('center_axis',(0.,0.,1.)) ;
#18131 = DIRECTION('ref_axis',(1.,0.,0.)) ;
#18132 = DIRECTION('',(0.,0.,-1.)) ;
#18133 = DIRECTION('center_axis',(0.,0.,-1.)) ;
#18134 = DIRECTION('ref_axis',(1.,0.,0.)) ;
#18135 = DIRECTION('',(0.,0.,-1.)) ;
#18136 = DIRECTION('center_axis',(-1.,0.,0.)) ;
#18137 = DIRECTION('ref_axis',(0.,0.,1.)) ;
#18138 = DIRECTION('',(0.,1.,0.)) ;
#18139 = DIRECTION('',(0.,-1.,0.)) ;
#18140 = DIRECTION('',(0.,0.,-1.)) ;
#18141 = DIRECTION('center_axis',(0.,0.,1.)) ;
#18142 = DIRECTION('ref_axis',(1.,0.,0.)) ;
#18143 = DIRECTION('center_axis',(0.,0.,1.)) ;
#18144 = DIRECTION('ref_axis',(1.,0.,0.)) ;
#18145 = DIRECTION('center_axis',(0.,0.,-1.)) ;
#18146 = DIRECTION('ref_axis',(1.,0.,0.)) ;
#18147 = DIRECTION('',(0.,0.,-1.)) ;
#18148 = DIRECTION('center_axis',(1.,0.,0.)) ;
#18149 = DIRECTION('ref_axis',(0.,0.,-1.)) ;
#18150 = DIRECTION('',(0.,-1.,0.)) ;
#18151 = DIRECTION('',(0.,1.,0.)) ;
#18152 = DIRECTION('center_axis',(0.,1.,0.)) ;
#18153 = DIRECTION('ref_axis',(1.,0.,0.)) ;
#18154 = DIRECTION('center_axis',(0.,1.,0.)) ;
#18155 = DIRECTION('ref_axis',(1.,0.,0.)) ;
#18156 = DIRECTION('',(0.,1.,0.)) ;
#18157 = DIRECTION('center_axis',(0.,-1.,0.)) ;
#18158 = DIRECTION('ref_axis',(1.,0.,0.)) ;
#18159 = DIRECTION('center_axis',(0.,0.,1.)) ;
#18160 = DIRECTION('ref_axis',(1.,0.,0.)) ;
#18161 = DIRECTION('',(1.,0.,0.)) ;
#18162 = DIRECTION('',(0.,1.,0.)) ;
#18163 = DIRECTION('',(1.,0.,0.)) ;
#18164 = DIRECTION('',(0.,-1.,0.)) ;
#18165 = DIRECTION('center_axis',(0.,-1.,0.)) ;
#18166 = DIRECTION('ref_axis',(0.,0.,-1.)) ;
#18167 = DIRECTION('',(0.,0.,-1.)) ;
#18168 = DIRECTION('',(0.,0.,-1.)) ;
#18169 = DIRECTION('',(-1.,0.,0.)) ;
#18170 = DIRECTION('center_axis',(0.,-1.,0.)) ;
#18171 = DIRECTION('ref_axis',(0.,0.,-1.)) ;
#18172 = DIRECTION('',(0.,0.,-1.)) ;
#18173 = DIRECTION('',(1.,0.,0.)) ;
#18174 = DIRECTION('',(0.,0.,-1.)) ;
#18175 = DIRECTION('center_axis',(-1.,0.,0.)) ;
#18176 = DIRECTION('ref_axis',(0.,0.,1.)) ;
#18177 = DIRECTION('',(0.,0.,-1.)) ;
#18178 = DIRECTION('',(0.,-1.,0.)) ;
#18179 = DIRECTION('',(0.,1.,0.)) ;
#18180 = DIRECTION('center_axis',(0.,0.,1.)) ;
#18181 = DIRECTION('ref_axis',(1.,0.,0.)) ;
#18182 = DIRECTION('',(0.,-1.,0.)) ;
#18183 = DIRECTION('',(1.,0.,0.)) ;
#18184 = DIRECTION('center_axis',(0.,0.,1.)) ;
#18185 = DIRECTION('ref_axis',(1.,0.,0.)) ;
#18186 = DIRECTION('',(-1.,0.,0.)) ;
#18187 = DIRECTION('',(0.,1.,0.)) ;
#18188 = DIRECTION('center_axis',(0.,1.,0.)) ;
#18189 = DIRECTION('ref_axis',(0.,0.,1.)) ;
#18190 = DIRECTION('',(0.,0.,-1.)) ;
#18191 = DIRECTION('center_axis',(1.,0.,0.)) ;
#18192 = DIRECTION('ref_axis',(0.,0.,-1.)) ;
#18193 = DIRECTION('',(0.,0.,1.)) ;
#18194 = DIRECTION('',(1.,0.,0.)) ;
#18195 = DIRECTION('',(0.,0.,1.)) ;
#18196 = DIRECTION('',(1.,0.,0.)) ;
#18197 = DIRECTION('',(0.,0.,1.)) ;
#18198 = DIRECTION('',(1.,0.,0.)) ;
#18199 = DIRECTION('',(0.,0.,1.)) ;
#18200 = DIRECTION('',(1.,0.,0.)) ;
#18201 = DIRECTION('',(0.,0.,1.)) ;
#18202 = DIRECTION('',(1.,0.,0.)) ;
#18203 = DIRECTION('',(0.,0.,1.)) ;
#18204 = DIRECTION('',(1.,0.,0.)) ;
#18205 = DIRECTION('',(0.,0.,1.)) ;
#18206 = DIRECTION('',(1.,0.,0.)) ;
#18207 = DIRECTION('',(0.,0.,1.)) ;
#18208 = DIRECTION('',(1.,0.,0.)) ;
#18209 = DIRECTION('',(0.,0.,1.)) ;
#18210 = DIRECTION('',(1.,0.,0.)) ;
#18211 = DIRECTION('',(0.,0.,1.)) ;
#18212 = DIRECTION('',(1.,0.,0.)) ;
#18213 = DIRECTION('',(0.,0.,1.)) ;
#18214 = DIRECTION('',(1.,0.,0.)) ;
#18215 = DIRECTION('',(0.,0.,1.)) ;
#18216 = DIRECTION('',(1.,0.,0.)) ;
#18217 = DIRECTION('',(0.,0.,1.)) ;
#18218 = DIRECTION('',(1.,0.,0.)) ;
#18219 = DIRECTION('',(-0.342020143325669,0.,0.939692620785908)) ;
#18220 = DIRECTION('',(0.939692620785908,0.,0.342020143325669)) ;
#18221 = DIRECTION('',(0.939692620785908,0.,0.342020143325669)) ;
#18222 = DIRECTION('',(0.342020143325669,0.,-0.939692620785908)) ;
#18223 = DIRECTION('',(-0.939692620785908,0.,-0.342020143325669)) ;
#18224 = DIRECTION('',(-0.342020143325669,0.,0.939692620785908)) ;
#18225 = DIRECTION('',(0.342020143325669,0.,-0.939692620785908)) ;
#18226 = DIRECTION('',(-0.939692620785908,0.,-0.342020143325669)) ;
#18227 = DIRECTION('',(0.,0.,1.)) ;
#18228 = DIRECTION('',(1.,0.,0.)) ;
#18229 = DIRECTION('',(0.,0.,1.)) ;
#18230 = DIRECTION('',(1.,0.,0.)) ;
#18231 = DIRECTION('',(0.,0.,1.)) ;
#18232 = DIRECTION('',(1.,0.,0.)) ;
#18233 = DIRECTION('',(0.,0.,1.)) ;
#18234 = DIRECTION('',(1.,0.,0.)) ;
#18235 = DIRECTION('',(0.,0.,1.)) ;
#18236 = DIRECTION('',(1.,0.,0.)) ;
#18237 = DIRECTION('axis',(0.,0.,1.)) ;
#18238 = DIRECTION('refdir',(1.,0.,0.)) ;
#18239 = DIRECTION('axis',(0.,0.,1.)) ;
#18240 = DIRECTION('refdir',(1.,0.,0.)) ;
#18241 = DIRECTION('center_axis',(0.,0.,1.)) ;
#18242 = DIRECTION('ref_axis',(1.,0.,0.)) ;
#18243 = DIRECTION('center_axis',(0.,0.,1.)) ;
#18244 = DIRECTION('ref_axis',(1.,0.,0.)) ;
#18245 = DIRECTION('center_axis',(0.,0.,1.)) ;
#18246 = DIRECTION('ref_axis',(1.,0.,0.)) ;
#18247 = DIRECTION('center_axis',(0.,0.,1.)) ;
#18248 = DIRECTION('ref_axis',(1.,0.,0.)) ;
#18249 = DIRECTION('center_axis',(0.,0.,1.)) ;
#18250 = DIRECTION('ref_axis',(1.,0.,0.)) ;
#18251 = DIRECTION('center_axis',(0.,0.,1.)) ;
#18252 = DIRECTION('ref_axis',(1.,0.,0.)) ;
#18253 = DIRECTION('',(0.,-1.,0.)) ;
#18254 = DIRECTION('',(1.,0.,0.)) ;
#18255 = DIRECTION('',(0.,1.,0.)) ;
#18256 = DIRECTION('',(-1.,-6.34413156928661E-17,0.)) ;
#18257 = DIRECTION('',(0.338445472540165,-0.290096119320142,-0.895153005732796)) ;
#18258 = DIRECTION('',(0.338445472540165,0.290096119320142,-0.895153005732796)) ;
#18259 = DIRECTION('',(-0.338445472540165,0.290096119320142,-0.895153005732796)) ;
#18260 = DIRECTION('',(-0.338445472540165,-0.290096119320142,-0.895153005732796)) ;
#18261 = DIRECTION('axis',(0.,0.,1.)) ;
#18262 = DIRECTION('refdir',(1.,0.,0.)) ;
#18263 = DIRECTION('center_axis',(0.,0.,1.)) ;
#18264 = DIRECTION('ref_axis',(1.,0.,0.)) ;
#18265 = DIRECTION('center_axis',(0.,0.,1.)) ;
#18266 = DIRECTION('ref_axis',(1.,0.,0.)) ;
#18267 = DIRECTION('',(0.,0.,-1.)) ;
#18268 = DIRECTION('center_axis',(0.,0.,-1.)) ;
#18269 = DIRECTION('ref_axis',(1.,0.,0.)) ;
#18270 = DIRECTION('center_axis',(0.,0.,1.)) ;
#18271 = DIRECTION('ref_axis',(1.,0.,0.)) ;
#18272 = DIRECTION('center_axis',(0.,-1.,0.)) ;
#18273 = DIRECTION('ref_axis',(0.,0.,-1.)) ;
#18274 = DIRECTION('',(-1.,0.,0.)) ;
#18275 = DIRECTION('',(0.,0.,-1.)) ;
#18276 = DIRECTION('',(-1.,0.,0.)) ;
#18277 = DIRECTION('',(0.,0.,-1.)) ;
#18278 = DIRECTION('center_axis',(1.,0.,0.)) ;
#18279 = DIRECTION('ref_axis',(0.,0.,-1.)) ;
#18280 = DIRECTION('',(0.,-1.,0.)) ;
#18281 = DIRECTION('',(0.,-1.,0.)) ;
#18282 = DIRECTION('',(0.,0.,-1.)) ;
#18283 = DIRECTION('center_axis',(0.,0.,1.)) ;
#18284 = DIRECTION('ref_axis',(1.,0.,0.)) ;
#18285 = DIRECTION('',(0.,1.,0.)) ;
#18286 = DIRECTION('',(1.,0.,0.)) ;
#18287 = DIRECTION('center_axis',(0.,1.,0.)) ;
#18288 = DIRECTION('ref_axis',(0.,0.,1.)) ;
#18289 = DIRECTION('',(1.,0.,0.)) ;
#18290 = DIRECTION('',(0.,0.,-1.)) ;
#18291 = DIRECTION('center_axis',(-1.,0.,0.)) ;
#18292 = DIRECTION('ref_axis',(0.,0.,1.)) ;
#18293 = DIRECTION('',(0.,1.,0.)) ;
#18294 = DIRECTION('center_axis',(0.,0.,1.)) ;
#18295 = DIRECTION('ref_axis',(1.,0.,0.)) ;
#18296 = DIRECTION('',(0.,-1.,0.)) ;
#18297 = DIRECTION('',(-1.,0.,0.)) ;
#18298 = DIRECTION('',(0.,1.,0.)) ;
#18299 = DIRECTION('',(1.,0.,0.)) ;
#18300 = DIRECTION('center_axis',(0.,1.,0.)) ;
#18301 = DIRECTION('ref_axis',(0.,0.,1.)) ;
#18302 = DIRECTION('',(0.,0.,-1.)) ;
#18303 = DIRECTION('',(0.,0.,-1.)) ;
#18304 = DIRECTION('',(1.,0.,0.)) ;
#18305 = DIRECTION('center_axis',(1.,0.,0.)) ;
#18306 = DIRECTION('ref_axis',(0.,0.,-1.)) ;
#18307 = DIRECTION('',(0.,0.,-1.)) ;
#18308 = DIRECTION('',(0.,-1.,0.)) ;
#18309 = DIRECTION('center_axis',(0.,-1.,0.)) ;
#18310 = DIRECTION('ref_axis',(0.,0.,-1.)) ;
#18311 = DIRECTION('',(0.,0.,-1.)) ;
#18312 = DIRECTION('',(-1.,0.,0.)) ;
#18313 = DIRECTION('center_axis',(-1.,0.,0.)) ;
#18314 = DIRECTION('ref_axis',(0.,0.,1.)) ;
#18315 = DIRECTION('',(0.,1.,0.)) ;
#18316 = DIRECTION('center_axis',(0.,0.,1.)) ;
#18317 = DIRECTION('ref_axis',(1.,0.,0.)) ;
#18318 = DIRECTION('',(0.,1.,0.)) ;
#18319 = DIRECTION('',(-1.,0.,0.)) ;
#18320 = DIRECTION('',(0.,-1.,0.)) ;
#18321 = DIRECTION('',(1.,0.,0.)) ;
#18322 = DIRECTION('center_axis',(0.,0.,1.)) ;
#18323 = DIRECTION('ref_axis',(1.,0.,0.)) ;
#18324 = DIRECTION('',(0.,-1.,0.)) ;
#18325 = DIRECTION('',(-1.,0.,0.)) ;
#18326 = DIRECTION('',(0.,1.,0.)) ;
#18327 = DIRECTION('',(1.,0.,0.)) ;
#18328 = DIRECTION('center_axis',(0.,1.,0.)) ;
#18329 = DIRECTION('ref_axis',(0.,0.,1.)) ;
#18330 = DIRECTION('',(0.,0.,-1.)) ;
#18331 = DIRECTION('',(0.,0.,-1.)) ;
#18332 = DIRECTION('center_axis',(1.,0.,0.)) ;
#18333 = DIRECTION('ref_axis',(0.,0.,-1.)) ;
#18334 = DIRECTION('',(0.,0.,-1.)) ;
#18335 = DIRECTION('center_axis',(0.,-1.,0.)) ;
#18336 = DIRECTION('ref_axis',(0.,0.,-1.)) ;
#18337 = DIRECTION('',(0.,0.,-1.)) ;
#18338 = DIRECTION('center_axis',(-1.,0.,0.)) ;
#18339 = DIRECTION('ref_axis',(0.,0.,1.)) ;
#18340 = DIRECTION('axis',(0.,0.,1.)) ;
#18341 = DIRECTION('refdir',(1.,0.,0.)) ;
#18342 = DIRECTION('center_axis',(1.,0.,0.)) ;
#18343 = DIRECTION('ref_axis',(0.,0.,-1.)) ;
#18344 = DIRECTION('',(0.,0.,-1.)) ;
#18345 = DIRECTION('',(0.,-1.,0.)) ;
#18346 = DIRECTION('',(0.,0.,-1.)) ;
#18347 = DIRECTION('',(0.,1.,0.)) ;
#18348 = DIRECTION('',(0.,0.,-1.)) ;
#18349 = DIRECTION('',(0.,-1.,0.)) ;
#18350 = DIRECTION('',(0.,0.,1.)) ;
#18351 = DIRECTION('',(0.,1.,0.)) ;
#18352 = DIRECTION('center_axis',(0.,0.,1.)) ;
#18353 = DIRECTION('ref_axis',(1.,0.,0.)) ;
#18354 = DIRECTION('',(0.,1.,0.)) ;
#18355 = DIRECTION('',(-1.,0.,0.)) ;
#18356 = DIRECTION('',(0.,-1.,0.)) ;
#18357 = DIRECTION('',(1.,0.,0.)) ;
#18358 = DIRECTION('center_axis',(0.,1.,0.)) ;
#18359 = DIRECTION('ref_axis',(0.,0.,1.)) ;
#18360 = DIRECTION('center_axis',(0.,1.,0.)) ;
#18361 = DIRECTION('ref_axis',(1.,0.,0.)) ;
#18362 = DIRECTION('',(-1.,0.,0.)) ;
#18363 = DIRECTION('',(0.,0.,-1.)) ;
#18364 = DIRECTION('',(1.,0.,0.)) ;
#18365 = DIRECTION('',(0.,0.,-1.)) ;
#18366 = DIRECTION('center_axis',(0.,-1.,0.)) ;
#18367 = DIRECTION('ref_axis',(0.,0.,-1.)) ;
#18368 = DIRECTION('center_axis',(0.,-1.,0.)) ;
#18369 = DIRECTION('ref_axis',(1.,0.,0.)) ;
#18370 = DIRECTION('',(0.,0.,-1.)) ;
#18371 = DIRECTION('',(-1.,0.,0.)) ;
#18372 = DIRECTION('',(0.,0.,1.)) ;
#18373 = DIRECTION('',(1.,0.,0.)) ;
#18374 = DIRECTION('center_axis',(0.,-1.,0.)) ;
#18375 = DIRECTION('ref_axis',(0.,0.,-1.)) ;
#18376 = DIRECTION('',(0.,0.,-1.)) ;
#18377 = DIRECTION('',(-1.,0.,0.)) ;
#18378 = DIRECTION('',(1.,0.,0.)) ;
#18379 = DIRECTION('center_axis',(0.,-1.,0.)) ;
#18380 = DIRECTION('ref_axis',(1.,0.,0.)) ;
#18381 = DIRECTION('',(1.,0.,0.)) ;
#18382 = DIRECTION('center_axis',(0.,0.,1.)) ;
#18383 = DIRECTION('ref_axis',(1.,0.,0.)) ;
#18384 = DIRECTION('center_axis',(0.,0.,-1.)) ;
#18385 = DIRECTION('ref_axis',(1.,0.,0.)) ;
#18386 = DIRECTION('',(0.,1.,0.)) ;
#18387 = DIRECTION('center_axis',(0.,0.,1.)) ;
#18388 = DIRECTION('ref_axis',(1.,0.,0.)) ;
#18389 = DIRECTION('center_axis',(0.,0.,-1.)) ;
#18390 = DIRECTION('ref_axis',(1.,0.,0.)) ;
#18391 = DIRECTION('center_axis',(0.,0.,1.)) ;
#18392 = DIRECTION('ref_axis',(1.,0.,0.)) ;
#18393 = DIRECTION('center_axis',(0.,0.,-1.)) ;
#18394 = DIRECTION('ref_axis',(1.,0.,0.)) ;
#18395 = DIRECTION('',(0.,1.,0.)) ;
#18396 = DIRECTION('center_axis',(0.,0.,1.)) ;
#18397 = DIRECTION('ref_axis',(1.,0.,0.)) ;
#18398 = DIRECTION('center_axis',(0.,0.,-1.)) ;
#18399 = DIRECTION('ref_axis',(1.,0.,0.)) ;
#18400 = DIRECTION('',(1.,0.,0.)) ;
#18401 = DIRECTION('center_axis',(0.,0.,1.)) ;
#18402 = DIRECTION('ref_axis',(1.,0.,0.)) ;
#18403 = DIRECTION('',(0.,-1.,0.)) ;
#18404 = DIRECTION('',(-1.,0.,0.)) ;
#18405 = DIRECTION('center_axis',(0.,1.,0.)) ;
#18406 = DIRECTION('ref_axis',(0.,0.,1.)) ;
#18407 = DIRECTION('',(0.,0.,1.)) ;
#18408 = DIRECTION('',(-1.,0.,0.)) ;
#18409 = DIRECTION('center_axis',(0.,1.,0.)) ;
#18410 = DIRECTION('ref_axis',(1.,0.,0.)) ;
#18411 = DIRECTION('center_axis',(-1.,0.,0.)) ;
#18412 = DIRECTION('ref_axis',(0.,0.,1.)) ;
#18413 = DIRECTION('',(0.,0.,1.)) ;
#18414 = DIRECTION('',(0.,-1.,0.)) ;
#18415 = DIRECTION('',(0.,0.,-1.)) ;
#18416 = DIRECTION('center_axis',(0.,0.,-1.)) ;
#18417 = DIRECTION('ref_axis',(-1.,0.,0.)) ;
#18418 = DIRECTION('',(0.,1.,0.)) ;
#18419 = DIRECTION('center_axis',(0.,0.,-1.)) ;
#18420 = DIRECTION('ref_axis',(1.,0.,0.)) ;
#18421 = DIRECTION('center_axis',(0.,0.,-1.)) ;
#18422 = DIRECTION('ref_axis',(-1.,0.,0.)) ;
#18423 = DIRECTION('center_axis',(0.,0.,-1.)) ;
#18424 = DIRECTION('ref_axis',(1.,0.,0.)) ;
#18425 = DIRECTION('',(0.,1.,0.)) ;
#18426 = DIRECTION('center_axis',(0.,0.,-1.)) ;
#18427 = DIRECTION('ref_axis',(-1.,0.,0.)) ;
#18428 = DIRECTION('center_axis',(0.,0.,-1.)) ;
#18429 = DIRECTION('ref_axis',(1.,0.,0.)) ;
#18430 = DIRECTION('center_axis',(0.,0.,-1.)) ;
#18431 = DIRECTION('ref_axis',(1.,0.,0.)) ;
#18432 = DIRECTION('center_axis',(0.,0.,-1.)) ;
#18433 = DIRECTION('ref_axis',(-1.,0.,0.)) ;
#18434 = DIRECTION('center_axis',(0.,0.,-1.)) ;
#18435 = DIRECTION('ref_axis',(1.,0.,0.)) ;
#18436 = DIRECTION('',(0.,-1.,0.)) ;
#18437 = DIRECTION('center_axis',(0.,0.,-1.)) ;
#18438 = DIRECTION('ref_axis',(-1.,0.,0.)) ;
#18439 = DIRECTION('center_axis',(0.,0.,-1.)) ;
#18440 = DIRECTION('ref_axis',(1.,0.,0.)) ;
#18441 = DIRECTION('center_axis',(0.,0.,1.)) ;
#18442 = DIRECTION('ref_axis',(1.,0.,0.)) ;
#18443 = DIRECTION('center_axis',(0.,0.,1.)) ;
#18444 = DIRECTION('ref_axis',(1.,0.,0.)) ;
#18445 = DIRECTION('',(0.,0.,1.)) ;
#18446 = DIRECTION('center_axis',(0.,1.,0.)) ;
#18447 = DIRECTION('ref_axis',(1.,0.,0.)) ;
#18448 = DIRECTION('center_axis',(0.,1.,0.)) ;
#18449 = DIRECTION('ref_axis',(1.,0.,0.)) ;
#18450 = DIRECTION('',(0.,1.,0.)) ;
#18451 = DIRECTION('center_axis',(0.,-1.,0.)) ;
#18452 = DIRECTION('ref_axis',(1.,0.,0.)) ;
#18453 = DIRECTION('center_axis',(0.,1.,0.)) ;
#18454 = DIRECTION('ref_axis',(1.,0.,0.)) ;
#18455 = DIRECTION('center_axis',(0.,1.,0.)) ;
#18456 = DIRECTION('ref_axis',(1.,0.,0.)) ;
#18457 = DIRECTION('',(0.,1.,0.)) ;
#18458 = DIRECTION('center_axis',(0.,-1.,0.)) ;
#18459 = DIRECTION('ref_axis',(1.,0.,0.)) ;
#18460 = DIRECTION('center_axis',(0.,1.,0.)) ;
#18461 = DIRECTION('ref_axis',(1.,0.,0.)) ;
#18462 = DIRECTION('center_axis',(0.,-1.,0.)) ;
#18463 = DIRECTION('ref_axis',(1.,0.,0.)) ;
#18464 = DIRECTION('',(0.,1.,0.)) ;
#18465 = DIRECTION('center_axis',(0.,1.,0.)) ;
#18466 = DIRECTION('ref_axis',(1.,0.,0.)) ;
#18467 = DIRECTION('',(0.,-1.,0.)) ;
#18468 = DIRECTION('center_axis',(0.,-1.,0.)) ;
#18469 = DIRECTION('ref_axis',(-1.,0.,0.)) ;
#18470 = DIRECTION('center_axis',(0.,1.,0.)) ;
#18471 = DIRECTION('ref_axis',(1.,0.,0.)) ;
#18472 = DIRECTION('center_axis',(0.,0.,-1.)) ;
#18473 = DIRECTION('ref_axis',(-1.,0.,0.)) ;
#18474 = DIRECTION('center_axis',(0.,0.,-1.)) ;
#18475 = DIRECTION('ref_axis',(1.,0.,0.)) ;
#18476 = DIRECTION('center_axis',(0.,0.,1.)) ;
#18477 = DIRECTION('ref_axis',(1.,0.,0.)) ;
#18478 = DIRECTION('',(0.,0.,1.)) ;
#18479 = DIRECTION('center_axis',(0.,0.,-1.)) ;
#18480 = DIRECTION('ref_axis',(1.,0.,0.)) ;
#18481 = DIRECTION('center_axis',(0.,0.,1.)) ;
#18482 = DIRECTION('ref_axis',(1.,0.,0.)) ;
#18483 = DIRECTION('',(0.,1.,0.)) ;
#18484 = DIRECTION('',(-1.,0.,0.)) ;
#18485 = DIRECTION('',(0.,-1.,0.)) ;
#18486 = DIRECTION('',(1.,0.,0.)) ;
#18487 = DIRECTION('center_axis',(0.,0.,1.)) ;
#18488 = DIRECTION('ref_axis',(1.,0.,0.)) ;
#18489 = DIRECTION('',(0.,-1.,0.)) ;
#18490 = DIRECTION('',(-1.,0.,0.)) ;
#18491 = DIRECTION('',(0.,1.,0.)) ;
#18492 = DIRECTION('',(1.,0.,0.)) ;
#18493 = DIRECTION('center_axis',(0.,1.,0.)) ;
#18494 = DIRECTION('ref_axis',(0.,0.,1.)) ;
#18495 = DIRECTION('',(0.,0.,-1.)) ;
#18496 = DIRECTION('',(0.,0.,-1.)) ;
#18497 = DIRECTION('center_axis',(1.,0.,0.)) ;
#18498 = DIRECTION('ref_axis',(0.,0.,-1.)) ;
#18499 = DIRECTION('',(0.,0.,-1.)) ;
#18500 = DIRECTION('center_axis',(0.,-1.,0.)) ;
#18501 = DIRECTION('ref_axis',(0.,0.,-1.)) ;
#18502 = DIRECTION('',(0.,0.,-1.)) ;
#18503 = DIRECTION('center_axis',(-1.,0.,0.)) ;
#18504 = DIRECTION('ref_axis',(0.,0.,1.)) ;
#18505 = DIRECTION('axis',(0.,0.,1.)) ;
#18506 = DIRECTION('refdir',(1.,0.,0.)) ;
#18507 = DIRECTION('center_axis',(0.,1.,0.)) ;
#18508 = DIRECTION('ref_axis',(1.,0.,0.)) ;
#18509 = DIRECTION('center_axis',(0.,1.,0.)) ;
#18510 = DIRECTION('ref_axis',(1.,0.,0.)) ;
#18511 = DIRECTION('',(0.,1.,0.)) ;
#18512 = DIRECTION('center_axis',(0.,-1.,0.)) ;
#18513 = DIRECTION('ref_axis',(1.,0.,0.)) ;
#18514 = DIRECTION('center_axis',(0.,1.,0.)) ;
#18515 = DIRECTION('ref_axis',(-0.707106781186545,0.,0.70710678118655)) ;
#18516 = DIRECTION('center_axis',(0.,1.,0.)) ;
#18517 = DIRECTION('ref_axis',(1.,0.,0.)) ;
#18518 = DIRECTION('',(0.,-1.,0.)) ;
#18519 = DIRECTION('center_axis',(0.,-1.,0.)) ;
#18520 = DIRECTION('ref_axis',(1.,0.,0.)) ;
#18521 = DIRECTION('',(0.,1.,0.)) ;
#18522 = DIRECTION('center_axis',(0.,1.,0.)) ;
#18523 = DIRECTION('ref_axis',(1.,0.,0.)) ;
#18524 = DIRECTION('center_axis',(0.,1.,0.)) ;
#18525 = DIRECTION('ref_axis',(1.,0.,0.)) ;
#18526 = DIRECTION('center_axis',(0.,-1.,0.)) ;
#18527 = DIRECTION('ref_axis',(1.,0.,0.)) ;
#18528 = DIRECTION('center_axis',(0.,1.,0.)) ;
#18529 = DIRECTION('ref_axis',(1.,0.,0.)) ;
#18530 = DIRECTION('center_axis',(0.,-1.,0.)) ;
#18531 = DIRECTION('ref_axis',(1.,0.,0.)) ;
#18532 = DIRECTION('center_axis',(0.,1.,0.)) ;
#18533 = DIRECTION('ref_axis',(1.,0.,0.)) ;
#18534 = DIRECTION('center_axis',(0.,-1.,0.)) ;
#18535 = DIRECTION('ref_axis',(1.,0.,0.)) ;
#18536 = DIRECTION('center_axis',(0.,1.,0.)) ;
#18537 = DIRECTION('ref_axis',(1.,0.,0.)) ;
#18538 = DIRECTION('center_axis',(0.,-1.,0.)) ;
#18539 = DIRECTION('ref_axis',(1.,0.,0.)) ;
#18540 = DIRECTION('center_axis',(0.,1.,0.)) ;
#18541 = DIRECTION('ref_axis',(1.,0.,0.)) ;
#18542 = DIRECTION('center_axis',(0.,-1.,0.)) ;
#18543 = DIRECTION('ref_axis',(1.,0.,0.)) ;
#18544 = DIRECTION('center_axis',(0.,1.,0.)) ;
#18545 = DIRECTION('ref_axis',(1.,0.,0.)) ;
#18546 = DIRECTION('center_axis',(0.,-1.,0.)) ;
#18547 = DIRECTION('ref_axis',(1.,0.,0.)) ;
#18548 = DIRECTION('center_axis',(0.,1.,0.)) ;
#18549 = DIRECTION('ref_axis',(1.,0.,0.)) ;
#18550 = DIRECTION('center_axis',(0.,-1.,0.)) ;
#18551 = DIRECTION('ref_axis',(1.,0.,0.)) ;
#18552 = DIRECTION('center_axis',(0.,1.,0.)) ;
#18553 = DIRECTION('ref_axis',(1.,0.,0.)) ;
#18554 = DIRECTION('center_axis',(0.,1.,0.)) ;
#18555 = DIRECTION('ref_axis',(1.,0.,0.)) ;
#18556 = DIRECTION('center_axis',(0.,-1.,0.)) ;
#18557 = DIRECTION('ref_axis',(1.,0.,0.)) ;
#18558 = DIRECTION('',(0.,1.,0.)) ;
#18559 = DIRECTION('center_axis',(0.,1.,0.)) ;
#18560 = DIRECTION('ref_axis',(1.,0.,0.)) ;
#18561 = DIRECTION('center_axis',(0.,1.,0.)) ;
#18562 = DIRECTION('ref_axis',(1.,0.,0.)) ;
#18563 = DIRECTION('',(0.,-1.,0.)) ;
#18564 = DIRECTION('center_axis',(0.,1.,0.)) ;
#18565 = DIRECTION('ref_axis',(1.,0.,0.)) ;
#18566 = DIRECTION('center_axis',(0.,-1.,0.)) ;
#18567 = DIRECTION('ref_axis',(1.,0.,0.)) ;
#18568 = DIRECTION('',(0.,1.,0.)) ;
#18569 = DIRECTION('center_axis',(0.,1.,0.)) ;
#18570 = DIRECTION('ref_axis',(1.,0.,0.)) ;
#18571 = DIRECTION('center_axis',(0.,1.,0.)) ;
#18572 = DIRECTION('ref_axis',(1.,0.,0.)) ;
#18573 = DIRECTION('',(0.,-1.,0.)) ;
#18574 = DIRECTION('center_axis',(0.,1.,0.)) ;
#18575 = DIRECTION('ref_axis',(1.,0.,0.)) ;
#18576 = DIRECTION('center_axis',(0.,-1.,0.)) ;
#18577 = DIRECTION('ref_axis',(1.,0.,0.)) ;
#18578 = DIRECTION('',(0.,1.,0.)) ;
#18579 = DIRECTION('center_axis',(0.,1.,0.)) ;
#18580 = DIRECTION('ref_axis',(1.,0.,0.)) ;
#18581 = DIRECTION('center_axis',(0.,1.,0.)) ;
#18582 = DIRECTION('ref_axis',(1.,0.,0.)) ;
#18583 = DIRECTION('',(0.,-1.,0.)) ;
#18584 = DIRECTION('center_axis',(0.,1.,0.)) ;
#18585 = DIRECTION('ref_axis',(1.,0.,0.)) ;
#18586 = DIRECTION('center_axis',(0.,-1.,0.)) ;
#18587 = DIRECTION('ref_axis',(1.,0.,0.)) ;
#18588 = DIRECTION('',(0.,1.,0.)) ;
#18589 = DIRECTION('center_axis',(0.,1.,0.)) ;
#18590 = DIRECTION('ref_axis',(1.,0.,0.)) ;
#18591 = DIRECTION('center_axis',(0.,1.,0.)) ;
#18592 = DIRECTION('ref_axis',(1.,0.,0.)) ;
#18593 = DIRECTION('',(0.,-1.,0.)) ;
#18594 = DIRECTION('center_axis',(0.,1.,0.)) ;
#18595 = DIRECTION('ref_axis',(1.,0.,0.)) ;
#18596 = DIRECTION('center_axis',(0.,-1.,0.)) ;
#18597 = DIRECTION('ref_axis',(1.,0.,0.)) ;
#18598 = DIRECTION('',(0.,1.,0.)) ;
#18599 = DIRECTION('center_axis',(0.,1.,0.)) ;
#18600 = DIRECTION('ref_axis',(1.,0.,0.)) ;
#18601 = DIRECTION('center_axis',(0.,1.,0.)) ;
#18602 = DIRECTION('ref_axis',(1.,0.,0.)) ;
#18603 = DIRECTION('',(0.,-1.,0.)) ;
#18604 = DIRECTION('center_axis',(0.,1.,0.)) ;
#18605 = DIRECTION('ref_axis',(1.,0.,0.)) ;
#18606 = DIRECTION('center_axis',(0.,-1.,0.)) ;
#18607 = DIRECTION('ref_axis',(1.,0.,0.)) ;
#18608 = DIRECTION('',(0.,1.,0.)) ;
#18609 = DIRECTION('center_axis',(0.,1.,0.)) ;
#18610 = DIRECTION('ref_axis',(-0.707106781186545,0.,-0.70710678118655)) ;
#18611 = DIRECTION('center_axis',(0.,1.,0.)) ;
#18612 = DIRECTION('ref_axis',(1.,0.,0.)) ;
#18613 = DIRECTION('',(0.,-1.,0.)) ;
#18614 = DIRECTION('center_axis',(0.,1.,0.)) ;
#18615 = DIRECTION('ref_axis',(1.,0.,0.)) ;
#18616 = DIRECTION('center_axis',(0.,-1.,0.)) ;
#18617 = DIRECTION('ref_axis',(1.,0.,0.)) ;
#18618 = DIRECTION('',(0.,1.,0.)) ;
#18619 = DIRECTION('center_axis',(0.,1.,0.)) ;
#18620 = DIRECTION('ref_axis',(-1.,0.,1.22464679914735E-16)) ;
#18621 = DIRECTION('center_axis',(0.,1.,0.)) ;
#18622 = DIRECTION('ref_axis',(1.,0.,0.)) ;
#18623 = DIRECTION('',(0.,-1.,0.)) ;
#18624 = DIRECTION('center_axis',(0.,-1.,0.)) ;
#18625 = DIRECTION('ref_axis',(-1.,0.,0.)) ;
#18626 = DIRECTION('center_axis',(0.,-1.,0.)) ;
#18627 = DIRECTION('ref_axis',(1.,0.,0.)) ;
#18628 = DIRECTION('center_axis',(0.,1.,0.)) ;
#18629 = DIRECTION('ref_axis',(1.,0.,0.)) ;
#18630 = DIRECTION('axis',(0.,0.,1.)) ;
#18631 = DIRECTION('refdir',(1.,0.,0.)) ;
#18632 = DIRECTION('center_axis',(0.,1.,0.)) ;
#18633 = DIRECTION('ref_axis',(1.,0.,0.)) ;
#18634 = DIRECTION('center_axis',(0.,1.,0.)) ;
#18635 = DIRECTION('ref_axis',(1.,0.,0.)) ;
#18636 = DIRECTION('',(0.,-1.,0.)) ;
#18637 = DIRECTION('center_axis',(0.,-1.,0.)) ;
#18638 = DIRECTION('ref_axis',(1.,0.,0.)) ;
#18639 = DIRECTION('center_axis',(0.,-1.,0.)) ;
#18640 = DIRECTION('ref_axis',(-1.,0.,0.)) ;
#18641 = DIRECTION('center_axis',(0.,1.,0.)) ;
#18642 = DIRECTION('ref_axis',(1.,0.,0.)) ;
#18643 = DIRECTION('axis',(0.,0.,1.)) ;
#18644 = DIRECTION('refdir',(1.,0.,0.)) ;
#18645 = DIRECTION('center_axis',(0.,1.,0.)) ;
#18646 = DIRECTION('ref_axis',(1.,0.,0.)) ;
#18647 = DIRECTION('center_axis',(0.,1.,0.)) ;
#18648 = DIRECTION('ref_axis',(1.,0.,0.)) ;
#18649 = DIRECTION('',(0.,1.,0.)) ;
#18650 = DIRECTION('center_axis',(0.,-1.,0.)) ;
#18651 = DIRECTION('ref_axis',(1.,0.,0.)) ;
#18652 = DIRECTION('center_axis',(0.,1.,0.)) ;
#18653 = DIRECTION('ref_axis',(1.,0.,0.)) ;
#18654 = DIRECTION('center_axis',(0.,1.,0.)) ;
#18655 = DIRECTION('ref_axis',(1.,0.,0.)) ;
#18656 = DIRECTION('',(0.,-1.,0.)) ;
#18657 = DIRECTION('center_axis',(0.,-1.,0.)) ;
#18658 = DIRECTION('ref_axis',(1.,0.,0.)) ;
#18659 = DIRECTION('center_axis',(0.,-1.,0.)) ;
#18660 = DIRECTION('ref_axis',(-1.,0.,0.)) ;
#18661 = DIRECTION('center_axis',(0.,1.,0.)) ;
#18662 = DIRECTION('ref_axis',(1.,0.,0.)) ;
#18663 = DIRECTION('axis',(0.,0.,1.)) ;
#18664 = DIRECTION('refdir',(1.,0.,0.)) ;
#18665 = DIRECTION('center_axis',(0.,1.,0.)) ;
#18666 = DIRECTION('ref_axis',(1.,0.,0.)) ;
#18667 = DIRECTION('center_axis',(0.,1.,0.)) ;
#18668 = DIRECTION('ref_axis',(1.,0.,0.)) ;
#18669 = DIRECTION('',(0.,1.,0.)) ;
#18670 = DIRECTION('center_axis',(0.,-1.,0.)) ;
#18671 = DIRECTION('ref_axis',(1.,0.,0.)) ;
#18672 = DIRECTION('center_axis',(0.,1.,0.)) ;
#18673 = DIRECTION('ref_axis',(1.,0.,0.)) ;
#18674 = DIRECTION('center_axis',(0.,1.,0.)) ;
#18675 = DIRECTION('ref_axis',(1.,0.,0.)) ;
#18676 = DIRECTION('',(0.,-1.,0.)) ;
#18677 = DIRECTION('center_axis',(0.,-1.,0.)) ;
#18678 = DIRECTION('ref_axis',(1.,0.,0.)) ;
#18679 = DIRECTION('center_axis',(0.,-1.,0.)) ;
#18680 = DIRECTION('ref_axis',(-1.,0.,0.)) ;
#18681 = DIRECTION('center_axis',(0.,1.,0.)) ;
#18682 = DIRECTION('ref_axis',(0.587785252292473,0.,0.809016994374947)) ;
#18683 = DIRECTION('center_axis',(0.,-1.,0.)) ;
#18684 = DIRECTION('ref_axis',(1.,0.,0.)) ;
#18685 = DIRECTION('',(-0.809016994374947,0.,0.587785252292473)) ;
#18686 = DIRECTION('',(-0.587785252292473,0.,-0.809016994374947)) ;
#18687 = DIRECTION('',(0.809016994374947,0.,-0.587785252292473)) ;
#18688 = DIRECTION('center_axis',(0.587785252292473,0.,0.809016994374947)) ;
#18689 = DIRECTION('ref_axis',(0.809016994374947,0.,-0.587785252292473)) ;
#18690 = DIRECTION('',(0.,-1.,0.)) ;
#18691 = DIRECTION('',(0.809016994374947,0.,-0.587785252292473)) ;
#18692 = DIRECTION('',(0.,-1.,0.)) ;
#18693 = DIRECTION('center_axis',(0.587785252292473,0.,0.809016994374947)) ;
#18694 = DIRECTION('ref_axis',(0.809016994374947,0.,-0.587785252292473)) ;
#18695 = DIRECTION('',(0.,1.,0.)) ;
#18696 = DIRECTION('',(0.,1.,0.)) ;
#18697 = DIRECTION('',(-0.809016994374947,0.,0.587785252292473)) ;
#18698 = DIRECTION('center_axis',(0.,-1.,0.)) ;
#18699 = DIRECTION('ref_axis',(-0.587785252292473,0.,-0.809016994374947)) ;
#18700 = DIRECTION('center_axis',(0.,1.,0.)) ;
#18701 = DIRECTION('ref_axis',(1.,0.,0.)) ;
#18702 = DIRECTION('',(-0.587785252292473,0.,-0.809016994374947)) ;
#18703 = DIRECTION('center_axis',(-0.809016994374947,0.,0.587785252292473)) ;
#18704 = DIRECTION('ref_axis',(0.587785252292473,0.,0.809016994374947)) ;
#18705 = DIRECTION('center_axis',(0.,1.,0.)) ;
#18706 = DIRECTION('ref_axis',(0.951056516295154,0.,0.309016994374947)) ;
#18707 = DIRECTION('center_axis',(0.,-1.,0.)) ;
#18708 = DIRECTION('ref_axis',(1.,0.,0.)) ;
#18709 = DIRECTION('',(-0.309016994374947,0.,0.951056516295154)) ;
#18710 = DIRECTION('',(-0.951056516295154,0.,-0.309016994374947)) ;
#18711 = DIRECTION('',(0.309016994374947,0.,-0.951056516295154)) ;
#18712 = DIRECTION('center_axis',(0.951056516295154,0.,0.309016994374947)) ;
#18713 = DIRECTION('ref_axis',(0.309016994374947,0.,-0.951056516295154)) ;
#18714 = DIRECTION('',(0.,-1.,0.)) ;
#18715 = DIRECTION('',(0.309016994374947,0.,-0.951056516295154)) ;
#18716 = DIRECTION('',(0.,-1.,0.)) ;
#18717 = DIRECTION('center_axis',(0.951056516295154,0.,0.309016994374947)) ;
#18718 = DIRECTION('ref_axis',(0.309016994374947,0.,-0.951056516295154)) ;
#18719 = DIRECTION('',(0.,1.,0.)) ;
#18720 = DIRECTION('',(0.,1.,0.)) ;
#18721 = DIRECTION('',(-0.309016994374947,0.,0.951056516295154)) ;
#18722 = DIRECTION('center_axis',(0.,-1.,0.)) ;
#18723 = DIRECTION('ref_axis',(-0.951056516295154,0.,-0.309016994374947)) ;
#18724 = DIRECTION('center_axis',(0.,1.,0.)) ;
#18725 = DIRECTION('ref_axis',(1.,0.,0.)) ;
#18726 = DIRECTION('',(-0.951056516295154,0.,-0.309016994374947)) ;
#18727 = DIRECTION('center_axis',(-0.309016994374947,0.,0.951056516295154)) ;
#18728 = DIRECTION('ref_axis',(0.951056516295154,0.,0.309016994374947)) ;
#18729 = DIRECTION('center_axis',(0.,1.,0.)) ;
#18730 = DIRECTION('ref_axis',(0.951056516295154,0.,-0.309016994374948)) ;
#18731 = DIRECTION('center_axis',(0.,-1.,0.)) ;
#18732 = DIRECTION('ref_axis',(1.,0.,0.)) ;
#18733 = DIRECTION('',(0.309016994374948,0.,0.951056516295154)) ;
#18734 = DIRECTION('',(-0.951056516295154,0.,0.309016994374948)) ;
#18735 = DIRECTION('',(-0.309016994374948,0.,-0.951056516295154)) ;
#18736 = DIRECTION('center_axis',(0.951056516295154,0.,-0.309016994374948)) ;
#18737 = DIRECTION('ref_axis',(-0.309016994374948,0.,-0.951056516295154)) ;
#18738 = DIRECTION('',(0.,-1.,0.)) ;
#18739 = DIRECTION('',(-0.309016994374948,0.,-0.951056516295154)) ;
#18740 = DIRECTION('',(0.,-1.,0.)) ;
#18741 = DIRECTION('center_axis',(0.951056516295154,0.,-0.309016994374948)) ;
#18742 = DIRECTION('ref_axis',(-0.309016994374948,0.,-0.951056516295154)) ;
#18743 = DIRECTION('',(0.,1.,0.)) ;
#18744 = DIRECTION('',(0.,1.,0.)) ;
#18745 = DIRECTION('',(0.309016994374948,0.,0.951056516295154)) ;
#18746 = DIRECTION('center_axis',(0.,-1.,0.)) ;
#18747 = DIRECTION('ref_axis',(-0.951056516295154,0.,0.309016994374948)) ;
#18748 = DIRECTION('center_axis',(0.,1.,0.)) ;
#18749 = DIRECTION('ref_axis',(1.,0.,0.)) ;
#18750 = DIRECTION('',(-0.951056516295154,0.,0.309016994374948)) ;
#18751 = DIRECTION('center_axis',(0.309016994374948,0.,0.951056516295154)) ;
#18752 = DIRECTION('ref_axis',(0.951056516295154,0.,-0.309016994374948)) ;
#18753 = DIRECTION('center_axis',(0.,1.,0.)) ;
#18754 = DIRECTION('ref_axis',(0.587785252292473,0.,-0.809016994374948)) ;
#18755 = DIRECTION('center_axis',(0.,-1.,0.)) ;
#18756 = DIRECTION('ref_axis',(1.,0.,0.)) ;
#18757 = DIRECTION('',(0.809016994374948,0.,0.587785252292473)) ;
#18758 = DIRECTION('',(-0.587785252292473,0.,0.809016994374948)) ;
#18759 = DIRECTION('',(-0.809016994374948,0.,-0.587785252292473)) ;
#18760 = DIRECTION('center_axis',(0.587785252292473,0.,-0.809016994374948)) ;
#18761 = DIRECTION('ref_axis',(-0.809016994374948,0.,-0.587785252292473)) ;
#18762 = DIRECTION('',(0.,-1.,0.)) ;
#18763 = DIRECTION('',(-0.809016994374948,0.,-0.587785252292473)) ;
#18764 = DIRECTION('',(0.,-1.,0.)) ;
#18765 = DIRECTION('center_axis',(0.587785252292473,0.,-0.809016994374948)) ;
#18766 = DIRECTION('ref_axis',(-0.809016994374948,0.,-0.587785252292473)) ;
#18767 = DIRECTION('',(0.,1.,0.)) ;
#18768 = DIRECTION('',(0.,1.,0.)) ;
#18769 = DIRECTION('',(0.809016994374948,0.,0.587785252292473)) ;
#18770 = DIRECTION('center_axis',(0.,-1.,0.)) ;
#18771 = DIRECTION('ref_axis',(-0.587785252292473,0.,0.809016994374948)) ;
#18772 = DIRECTION('center_axis',(0.,1.,0.)) ;
#18773 = DIRECTION('ref_axis',(1.,0.,0.)) ;
#18774 = DIRECTION('',(-0.587785252292473,0.,0.809016994374948)) ;
#18775 = DIRECTION('center_axis',(0.809016994374948,0.,0.587785252292473)) ;
#18776 = DIRECTION('ref_axis',(0.587785252292473,0.,-0.809016994374948)) ;
#18777 = DIRECTION('center_axis',(0.,1.,0.)) ;
#18778 = DIRECTION('ref_axis',(-1.22464679914735E-16,0.,-1.)) ;
#18779 = DIRECTION('center_axis',(0.,-1.,0.)) ;
#18780 = DIRECTION('ref_axis',(1.,0.,0.)) ;
#18781 = DIRECTION('',(1.,0.,-1.22464679914735E-16)) ;
#18782 = DIRECTION('',(1.22464679914735E-16,0.,1.)) ;
#18783 = DIRECTION('',(-1.,0.,1.22464679914735E-16)) ;
#18784 = DIRECTION('center_axis',(0.,-1.,0.)) ;
#18785 = DIRECTION('ref_axis',(1.,0.,0.)) ;
#18786 = DIRECTION('center_axis',(-1.22464679914735E-16,0.,-1.)) ;
#18787 = DIRECTION('ref_axis',(-1.,0.,1.22464679914735E-16)) ;
#18788 = DIRECTION('',(0.,-1.,0.)) ;
#18789 = DIRECTION('',(-1.,0.,1.22464679914735E-16)) ;
#18790 = DIRECTION('',(0.,-1.,0.)) ;
#18791 = DIRECTION('center_axis',(-1.22464679914735E-16,0.,-1.)) ;
#18792 = DIRECTION('ref_axis',(-1.,0.,1.22464679914735E-16)) ;
#18793 = DIRECTION('',(0.,1.,0.)) ;
#18794 = DIRECTION('',(0.,1.,0.)) ;
#18795 = DIRECTION('',(1.,0.,-1.22464679914735E-16)) ;
#18796 = DIRECTION('center_axis',(0.,-1.,0.)) ;
#18797 = DIRECTION('ref_axis',(1.22464679914735E-16,0.,1.)) ;
#18798 = DIRECTION('center_axis',(0.,1.,0.)) ;
#18799 = DIRECTION('ref_axis',(1.,0.,0.)) ;
#18800 = DIRECTION('',(1.22464679914735E-16,0.,1.)) ;
#18801 = DIRECTION('center_axis',(0.,1.,0.)) ;
#18802 = DIRECTION('ref_axis',(1.,0.,0.)) ;
#18803 = DIRECTION('center_axis',(1.,0.,-1.22464679914735E-16)) ;
#18804 = DIRECTION('ref_axis',(-1.22464679914735E-16,0.,-1.)) ;
#18805 = DIRECTION('center_axis',(0.,1.,0.)) ;
#18806 = DIRECTION('ref_axis',(-0.587785252292473,0.,-0.809016994374947)) ;
#18807 = DIRECTION('center_axis',(0.,-1.,0.)) ;
#18808 = DIRECTION('ref_axis',(1.,0.,0.)) ;
#18809 = DIRECTION('',(0.809016994374947,0.,-0.587785252292473)) ;
#18810 = DIRECTION('',(0.587785252292473,0.,0.809016994374947)) ;
#18811 = DIRECTION('',(-0.809016994374947,0.,0.587785252292473)) ;
#18812 = DIRECTION('center_axis',(-0.587785252292473,0.,-0.809016994374947)) ;
#18813 = DIRECTION('ref_axis',(-0.809016994374947,0.,0.587785252292473)) ;
#18814 = DIRECTION('',(0.,-1.,0.)) ;
#18815 = DIRECTION('',(-0.809016994374947,0.,0.587785252292473)) ;
#18816 = DIRECTION('',(0.,-1.,0.)) ;
#18817 = DIRECTION('center_axis',(-0.587785252292473,0.,-0.809016994374947)) ;
#18818 = DIRECTION('ref_axis',(-0.809016994374947,0.,0.587785252292473)) ;
#18819 = DIRECTION('',(0.,1.,0.)) ;
#18820 = DIRECTION('',(0.,1.,0.)) ;
#18821 = DIRECTION('',(0.809016994374947,0.,-0.587785252292473)) ;
#18822 = DIRECTION('center_axis',(0.,-1.,0.)) ;
#18823 = DIRECTION('ref_axis',(0.587785252292473,0.,0.809016994374947)) ;
#18824 = DIRECTION('center_axis',(0.,1.,0.)) ;
#18825 = DIRECTION('ref_axis',(1.,0.,0.)) ;
#18826 = DIRECTION('',(0.587785252292473,0.,0.809016994374947)) ;
#18827 = DIRECTION('center_axis',(0.809016994374947,0.,-0.587785252292473)) ;
#18828 = DIRECTION('ref_axis',(-0.587785252292473,0.,-0.809016994374947)) ;
#18829 = DIRECTION('center_axis',(0.,1.,0.)) ;
#18830 = DIRECTION('ref_axis',(-0.951056516295154,0.,-0.309016994374947)) ;
#18831 = DIRECTION('center_axis',(0.,-1.,0.)) ;
#18832 = DIRECTION('ref_axis',(1.,0.,0.)) ;
#18833 = DIRECTION('',(0.309016994374947,0.,-0.951056516295154)) ;
#18834 = DIRECTION('',(0.951056516295154,0.,0.309016994374947)) ;
#18835 = DIRECTION('',(-0.309016994374947,0.,0.951056516295154)) ;
#18836 = DIRECTION('center_axis',(-0.951056516295154,0.,-0.309016994374947)) ;
#18837 = DIRECTION('ref_axis',(-0.309016994374947,0.,0.951056516295154)) ;
#18838 = DIRECTION('',(0.,-1.,0.)) ;
#18839 = DIRECTION('',(-0.309016994374947,0.,0.951056516295154)) ;
#18840 = DIRECTION('',(0.,-1.,0.)) ;
#18841 = DIRECTION('center_axis',(-0.951056516295154,0.,-0.309016994374947)) ;
#18842 = DIRECTION('ref_axis',(-0.309016994374947,0.,0.951056516295154)) ;
#18843 = DIRECTION('',(0.,1.,0.)) ;
#18844 = DIRECTION('',(0.,1.,0.)) ;
#18845 = DIRECTION('',(0.309016994374947,0.,-0.951056516295154)) ;
#18846 = DIRECTION('center_axis',(0.,-1.,0.)) ;
#18847 = DIRECTION('ref_axis',(0.951056516295154,0.,0.309016994374947)) ;
#18848 = DIRECTION('center_axis',(0.,1.,0.)) ;
#18849 = DIRECTION('ref_axis',(1.,0.,0.)) ;
#18850 = DIRECTION('',(0.951056516295154,0.,0.309016994374947)) ;
#18851 = DIRECTION('center_axis',(0.309016994374947,0.,-0.951056516295154)) ;
#18852 = DIRECTION('ref_axis',(-0.951056516295154,0.,-0.309016994374947)) ;
#18853 = DIRECTION('center_axis',(0.,1.,0.)) ;
#18854 = DIRECTION('ref_axis',(-0.951056516295154,0.,0.309016994374948)) ;
#18855 = DIRECTION('center_axis',(0.,-1.,0.)) ;
#18856 = DIRECTION('ref_axis',(1.,0.,0.)) ;
#18857 = DIRECTION('',(-0.309016994374948,0.,-0.951056516295154)) ;
#18858 = DIRECTION('',(0.951056516295154,0.,-0.309016994374948)) ;
#18859 = DIRECTION('',(0.309016994374948,0.,0.951056516295154)) ;
#18860 = DIRECTION('center_axis',(-0.951056516295154,0.,0.309016994374948)) ;
#18861 = DIRECTION('ref_axis',(0.309016994374948,0.,0.951056516295154)) ;
#18862 = DIRECTION('',(0.,-1.,0.)) ;
#18863 = DIRECTION('',(0.309016994374948,0.,0.951056516295154)) ;
#18864 = DIRECTION('',(0.,-1.,0.)) ;
#18865 = DIRECTION('center_axis',(-0.951056516295154,0.,0.309016994374948)) ;
#18866 = DIRECTION('ref_axis',(0.309016994374948,0.,0.951056516295154)) ;
#18867 = DIRECTION('',(0.,1.,0.)) ;
#18868 = DIRECTION('',(0.,1.,0.)) ;
#18869 = DIRECTION('',(-0.309016994374948,0.,-0.951056516295154)) ;
#18870 = DIRECTION('center_axis',(0.,-1.,0.)) ;
#18871 = DIRECTION('ref_axis',(0.951056516295154,0.,-0.309016994374948)) ;
#18872 = DIRECTION('center_axis',(0.,1.,0.)) ;
#18873 = DIRECTION('ref_axis',(1.,0.,0.)) ;
#18874 = DIRECTION('',(0.951056516295154,0.,-0.309016994374948)) ;
#18875 = DIRECTION('center_axis',(-0.309016994374948,0.,-0.951056516295154)) ;
#18876 = DIRECTION('ref_axis',(-0.951056516295154,0.,0.309016994374948)) ;
#18877 = DIRECTION('center_axis',(0.,1.,0.)) ;
#18878 = DIRECTION('ref_axis',(-0.587785252292473,0.,0.809016994374947)) ;
#18879 = DIRECTION('center_axis',(0.,-1.,0.)) ;
#18880 = DIRECTION('ref_axis',(1.,0.,0.)) ;
#18881 = DIRECTION('',(-0.809016994374947,0.,-0.587785252292473)) ;
#18882 = DIRECTION('',(0.587785252292473,0.,-0.809016994374947)) ;
#18883 = DIRECTION('',(0.809016994374947,0.,0.587785252292473)) ;
#18884 = DIRECTION('center_axis',(-0.587785252292473,0.,0.809016994374947)) ;
#18885 = DIRECTION('ref_axis',(0.809016994374947,0.,0.587785252292473)) ;
#18886 = DIRECTION('',(0.,-1.,0.)) ;
#18887 = DIRECTION('',(0.809016994374947,0.,0.587785252292473)) ;
#18888 = DIRECTION('',(0.,-1.,0.)) ;
#18889 = DIRECTION('center_axis',(-0.587785252292473,0.,0.809016994374947)) ;
#18890 = DIRECTION('ref_axis',(0.809016994374947,0.,0.587785252292473)) ;
#18891 = DIRECTION('',(0.,1.,0.)) ;
#18892 = DIRECTION('',(0.,1.,0.)) ;
#18893 = DIRECTION('',(-0.809016994374947,0.,-0.587785252292473)) ;
#18894 = DIRECTION('center_axis',(0.,-1.,0.)) ;
#18895 = DIRECTION('ref_axis',(0.587785252292473,0.,-0.809016994374947)) ;
#18896 = DIRECTION('center_axis',(0.,1.,0.)) ;
#18897 = DIRECTION('ref_axis',(1.,0.,0.)) ;
#18898 = DIRECTION('',(0.587785252292473,0.,-0.809016994374947)) ;
#18899 = DIRECTION('center_axis',(-0.809016994374947,0.,-0.587785252292473)) ;
#18900 = DIRECTION('ref_axis',(-0.587785252292473,0.,0.809016994374947)) ;
#18901 = DIRECTION('center_axis',(0.,1.,0.)) ;
#18902 = DIRECTION('ref_axis',(0.,0.,1.)) ;
#18903 = DIRECTION('center_axis',(0.,-1.,0.)) ;
#18904 = DIRECTION('ref_axis',(1.,0.,0.)) ;
#18905 = DIRECTION('',(-1.,0.,0.)) ;
#18906 = DIRECTION('',(0.,0.,-1.)) ;
#18907 = DIRECTION('',(1.,0.,0.)) ;
#18908 = DIRECTION('center_axis',(0.,0.,1.)) ;
#18909 = DIRECTION('ref_axis',(1.,0.,0.)) ;
#18910 = DIRECTION('',(0.,-1.,0.)) ;
#18911 = DIRECTION('',(1.,0.,0.)) ;
#18912 = DIRECTION('',(0.,-1.,0.)) ;
#18913 = DIRECTION('center_axis',(0.,0.,1.)) ;
#18914 = DIRECTION('ref_axis',(1.,0.,0.)) ;
#18915 = DIRECTION('',(0.,1.,0.)) ;
#18916 = DIRECTION('',(0.,1.,0.)) ;
#18917 = DIRECTION('',(-1.,0.,0.)) ;
#18918 = DIRECTION('center_axis',(0.,-1.,0.)) ;
#18919 = DIRECTION('ref_axis',(0.,0.,-1.)) ;
#18920 = DIRECTION('center_axis',(0.,1.,0.)) ;
#18921 = DIRECTION('ref_axis',(1.,0.,0.)) ;
#18922 = DIRECTION('',(0.,0.,-1.)) ;
#18923 = DIRECTION('center_axis',(-1.,0.,0.)) ;
#18924 = DIRECTION('ref_axis',(0.,0.,1.)) ;
#18925 = DIRECTION('center_axis',(0.,1.,0.)) ;
#18926 = DIRECTION('ref_axis',(1.,0.,0.)) ;
#18927 = DIRECTION('center_axis',(0.,1.,0.)) ;
#18928 = DIRECTION('ref_axis',(1.,0.,0.)) ;
#18929 = DIRECTION('',(0.,-1.,0.)) ;
#18930 = DIRECTION('',(0.,-1.,0.)) ;
#18931 = DIRECTION('center_axis',(0.,-1.,0.)) ;
#18932 = DIRECTION('ref_axis',(1.,0.,0.)) ;
#18933 = DIRECTION('center_axis',(0.,-1.,0.)) ;
#18934 = DIRECTION('ref_axis',(-1.,0.,0.)) ;
#18935 = DIRECTION('center_axis',(0.,1.,0.)) ;
#18936 = DIRECTION('ref_axis',(1.,0.,0.)) ;
#18937 = DIRECTION('axis',(0.,0.,1.)) ;
#18938 = DIRECTION('refdir',(1.,0.,0.)) ;
#18939 = DIRECTION('center_axis',(0.,0.,1.)) ;
#18940 = DIRECTION('ref_axis',(1.,0.,0.)) ;
#18941 = DIRECTION('center_axis',(0.,0.,1.)) ;
#18942 = DIRECTION('ref_axis',(1.,0.,0.)) ;
#18943 = DIRECTION('',(0.,0.,1.)) ;
#18944 = DIRECTION('center_axis',(0.,0.,-1.)) ;
#18945 = DIRECTION('ref_axis',(1.,0.,0.)) ;
#18946 = DIRECTION('center_axis',(0.,0.,1.)) ;
#18947 = DIRECTION('ref_axis',(1.,0.,0.)) ;
#18948 = DIRECTION('center_axis',(0.,0.,1.)) ;
#18949 = DIRECTION('ref_axis',(1.,0.,0.)) ;
#18950 = DIRECTION('',(0.,0.,-1.)) ;
#18951 = DIRECTION('center_axis',(0.,0.,-1.)) ;
#18952 = DIRECTION('ref_axis',(1.,0.,0.)) ;
#18953 = DIRECTION('center_axis',(0.,0.,-1.)) ;
#18954 = DIRECTION('ref_axis',(-1.,0.,0.)) ;
#18955 = DIRECTION('center_axis',(0.,0.,1.)) ;
#18956 = DIRECTION('ref_axis',(1.,0.,0.)) ;
#18957 = DIRECTION('axis',(0.,0.,1.)) ;
#18958 = DIRECTION('refdir',(1.,0.,0.)) ;
#18959 = DIRECTION('center_axis',(0.,-1.,0.)) ;
#18960 = DIRECTION('ref_axis',(-1.,0.,0.)) ;
#18961 = DIRECTION('',(-1.,0.,0.)) ;
#18962 = DIRECTION('center_axis',(0.,-1.,0.)) ;
#18963 = DIRECTION('ref_axis',(1.,0.,0.)) ;
#18964 = DIRECTION('',(-1.,0.,0.)) ;
#18965 = DIRECTION('center_axis',(0.,1.,0.)) ;
#18966 = DIRECTION('ref_axis',(1.,0.,0.)) ;
#18967 = DIRECTION('center_axis',(0.,1.,0.)) ;
#18968 = DIRECTION('ref_axis',(1.,0.,0.)) ;
#18969 = DIRECTION('center_axis',(0.,1.,0.)) ;
#18970 = DIRECTION('ref_axis',(1.,0.,0.)) ;
#18971 = DIRECTION('',(0.,-1.,0.)) ;
#18972 = DIRECTION('center_axis',(0.,-0.707106781186548,-0.707106781186548)) ;
#18973 = DIRECTION('ref_axis',(0.,0.707106781186547,-0.707106781186547)) ;
#18974 = DIRECTION('center_axis',(0.,1.,0.)) ;
#18975 = DIRECTION('ref_axis',(1.,0.,0.)) ;
#18976 = DIRECTION('',(0.,1.,0.)) ;
#18977 = DIRECTION('',(0.,-1.,0.)) ;
#18978 = DIRECTION('',(0.,1.,0.)) ;
#18979 = DIRECTION('center_axis',(0.,-1.,0.)) ;
#18980 = DIRECTION('ref_axis',(1.,0.,0.)) ;
#18981 = DIRECTION('center_axis',(0.,1.,0.)) ;
#18982 = DIRECTION('ref_axis',(1.,0.,0.)) ;
#18983 = DIRECTION('center_axis',(0.,0.,1.)) ;
#18984 = DIRECTION('ref_axis',(1.,0.,0.)) ;
#18985 = DIRECTION('center_axis',(0.,0.,1.)) ;
#18986 = DIRECTION('ref_axis',(1.,0.,0.)) ;
#18987 = DIRECTION('',(0.,0.,-1.)) ;
#18988 = DIRECTION('center_axis',(-0.707106781186548,0.,-0.707106781186547)) ;
#18989 = DIRECTION('ref_axis',(0.707106781186547,0.,-0.707106781186548)) ;
#18990 = DIRECTION('center_axis',(0.,0.,-1.)) ;
#18991 = DIRECTION('ref_axis',(1.,0.,0.)) ;
#18992 = DIRECTION('center_axis',(-0.707106781186548,0.,-0.707106781186547)) ;
#18993 = DIRECTION('ref_axis',(0.707106781186547,0.,-0.707106781186548)) ;
#18994 = DIRECTION('center_axis',(0.,0.,1.)) ;
#18995 = DIRECTION('ref_axis',(1.,0.,0.)) ;
#18996 = DIRECTION('center_axis',(0.,0.,1.)) ;
#18997 = DIRECTION('ref_axis',(1.,0.,0.)) ;
#18998 = DIRECTION('center_axis',(0.,0.,1.)) ;
#18999 = DIRECTION('ref_axis',(-1.,0.,0.)) ;
#19000 = DIRECTION('center_axis',(0.,0.,1.)) ;
#19001 = DIRECTION('ref_axis',(1.,0.,0.)) ;
#19002 = DIRECTION('center_axis',(0.577350269189627,0.577350269189626,0.577350269189625)) ;
#19003 = DIRECTION('ref_axis',(0.707106781186548,0.,-0.707106781186548)) ;
#19004 = DIRECTION('center_axis',(1.,0.,0.)) ;
#19005 = DIRECTION('ref_axis',(0.,0.,-1.)) ;
#19006 = DIRECTION('center_axis',(0.577350269189625,0.577350269189626,0.577350269189627)) ;
#19007 = DIRECTION('ref_axis',(-0.707106781186548,0.,0.707106781186547)) ;
#19008 = DIRECTION('center_axis',(-1.,0.,0.)) ;
#19009 = DIRECTION('ref_axis',(0.,0.,-1.)) ;
#19010 = DIRECTION('center_axis',(-0.408248290463863,0.816496580927726,-0.408248290463863)) ;
#19011 = DIRECTION('ref_axis',(0.707106781186548,0.,-0.707106781186547)) ;
#19012 = DIRECTION('center_axis',(-1.,0.,0.)) ;
#19013 = DIRECTION('ref_axis',(0.,0.,-1.)) ;
#19014 = DIRECTION('center_axis',(0.,-0.989949493661167,-0.141421356237309)) ;
#19015 = DIRECTION('ref_axis',(1.,0.,0.)) ;
#19016 = DIRECTION('center_axis',(0.,-0.989949493661167,-0.141421356237309)) ;
#19017 = DIRECTION('ref_axis',(1.,0.,0.)) ;
#19018 = DIRECTION('center_axis',(0.,0.,1.)) ;
#19019 = DIRECTION('ref_axis',(1.,0.,0.)) ;
#19020 = DIRECTION('center_axis',(0.,0.989949493661167,0.141421356237309)) ;
#19021 = DIRECTION('ref_axis',(1.,0.,0.)) ;
#19022 = DIRECTION('center_axis',(0.,0.,-1.)) ;
#19023 = DIRECTION('ref_axis',(1.,0.,0.)) ;
#19024 = DIRECTION('center_axis',(0.,0.,1.)) ;
#19025 = DIRECTION('ref_axis',(1.,0.,0.)) ;
#19026 = DIRECTION('center_axis',(1.,0.,0.)) ;
#19027 = DIRECTION('ref_axis',(0.,0.,-1.)) ;
#19028 = DIRECTION('',(-1.,0.,0.)) ;
#19029 = DIRECTION('center_axis',(-0.707106781186548,0.7,0.1)) ;
#19030 = DIRECTION('ref_axis',(-0.707106781186547,-0.7,-0.1)) ;
#19031 = DIRECTION('center_axis',(-0.707106781186548,0.7,0.1)) ;
#19032 = DIRECTION('ref_axis',(-0.707106781186547,-0.7,-0.1)) ;
#19033 = DIRECTION('center_axis',(0.,-0.989949493661167,-0.141421356237309)) ;
#19034 = DIRECTION('ref_axis',(1.,0.,0.)) ;
#19035 = DIRECTION('',(0.,0.989949493661167,0.141421356237309)) ;
#19036 = DIRECTION('center_axis',(0.,0.655201741360129,0.755453954995706)) ;
#19037 = DIRECTION('ref_axis',(0.,-0.755453954995706,0.655201741360129)) ;
#19038 = DIRECTION('center_axis',(0.,0.,1.)) ;
#19039 = DIRECTION('ref_axis',(1.,0.,0.)) ;
#19040 = DIRECTION('',(0.,0.,1.)) ;
#19041 = DIRECTION('center_axis',(0.,0.,-1.)) ;
#19042 = DIRECTION('ref_axis',(1.,0.,0.)) ;
#19043 = DIRECTION('center_axis',(0.,0.,1.)) ;
#19044 = DIRECTION('ref_axis',(1.,0.,0.)) ;
#19045 = DIRECTION('center_axis',(0.,0.,1.)) ;
#19046 = DIRECTION('ref_axis',(1.,0.,0.)) ;
#19047 = DIRECTION('',(0.,0.,-1.)) ;
#19048 = DIRECTION('center_axis',(0.,0.,1.)) ;
#19049 = DIRECTION('ref_axis',(1.,0.,0.)) ;
#19050 = DIRECTION('axis',(0.,0.,1.)) ;
#19051 = DIRECTION('refdir',(1.,0.,0.)) ;
#19052 = DIRECTION('center_axis',(0.,1.,0.)) ;
#19053 = DIRECTION('ref_axis',(0.,0.,1.)) ;
#19054 = DIRECTION('',(0.,0.,1.)) ;
#19055 = DIRECTION('',(-1.,0.,0.)) ;
#19056 = DIRECTION('',(0.,0.,-1.)) ;
#19057 = DIRECTION('',(1.,0.,0.)) ;
#19058 = DIRECTION('center_axis',(1.,0.,0.)) ;
#19059 = DIRECTION('ref_axis',(0.,0.,-1.)) ;
#19060 = DIRECTION('',(0.,0.,-1.)) ;
#19061 = DIRECTION('',(0.,-1.,0.)) ;
#19062 = DIRECTION('',(0.,0.,1.)) ;
#19063 = DIRECTION('',(0.,1.,0.)) ;
#19064 = DIRECTION('center_axis',(0.,-1.,0.)) ;
#19065 = DIRECTION('ref_axis',(0.,0.,-1.)) ;
#19066 = DIRECTION('',(0.,0.,-1.)) ;
#19067 = DIRECTION('',(-1.,0.,0.)) ;
#19068 = DIRECTION('',(0.,0.,-1.)) ;
#19069 = DIRECTION('',(1.,0.,0.)) ;
#19070 = DIRECTION('center_axis',(-1.,0.,0.)) ;
#19071 = DIRECTION('ref_axis',(0.,0.,1.)) ;
#19072 = DIRECTION('',(0.,-1.,0.)) ;
#19073 = DIRECTION('',(0.,1.,0.)) ;
#19074 = DIRECTION('center_axis',(0.,0.,-1.)) ;
#19075 = DIRECTION('ref_axis',(-1.,0.,0.)) ;
#19076 = DIRECTION('center_axis',(0.,0.,-1.)) ;
#19077 = DIRECTION('ref_axis',(1.,0.,0.)) ;
#19078 = DIRECTION('center_axis',(0.,0.,1.)) ;
#19079 = DIRECTION('ref_axis',(1.,0.,0.)) ;
#19080 = DIRECTION('center_axis',(0.,0.,1.)) ;
#19081 = DIRECTION('ref_axis',(-1.,-1.22464679914735E-16,0.)) ;
#19082 = DIRECTION('center_axis',(0.,0.,-1.)) ;
#19083 = DIRECTION('ref_axis',(1.,0.,0.)) ;
#19084 = DIRECTION('center_axis',(0.,0.,1.)) ;
#19085 = DIRECTION('ref_axis',(-1.,-1.22464679914735E-16,0.)) ;
#19086 = DIRECTION('center_axis',(0.,0.,1.)) ;
#19087 = DIRECTION('ref_axis',(1.,0.,0.)) ;
#19088 = DIRECTION('center_axis',(0.,0.,1.)) ;
#19089 = DIRECTION('ref_axis',(1.,0.,0.)) ;
#19090 = DIRECTION('axis',(0.,0.,1.)) ;
#19091 = DIRECTION('refdir',(1.,0.,0.)) ;
#19092 = DIRECTION('center_axis',(0.,0.,1.)) ;
#19093 = DIRECTION('ref_axis',(1.,0.,0.)) ;
#19094 = DIRECTION('',(0.,1.,0.)) ;
#19095 = DIRECTION('',(1.,0.,0.)) ;
#19096 = DIRECTION('',(0.,1.,0.)) ;
#19097 = DIRECTION('',(-1.,0.,0.)) ;
#19098 = DIRECTION('center_axis',(1.,0.,0.)) ;
#19099 = DIRECTION('ref_axis',(0.,0.,-1.)) ;
#19100 = DIRECTION('',(0.,1.,0.)) ;
#19101 = DIRECTION('',(0.,0.,-1.)) ;
#19102 = DIRECTION('',(0.,-1.,0.)) ;
#19103 = DIRECTION('',(0.,0.,-1.)) ;
#19104 = DIRECTION('center_axis',(0.,0.,1.)) ;
#19105 = DIRECTION('ref_axis',(1.,0.,0.)) ;
#19106 = DIRECTION('',(0.,-1.,0.)) ;
#19107 = DIRECTION('',(1.,0.,0.)) ;
#19108 = DIRECTION('',(0.,-1.,0.)) ;
#19109 = DIRECTION('',(-1.,0.,0.)) ;
#19110 = DIRECTION('center_axis',(-1.,0.,0.)) ;
#19111 = DIRECTION('ref_axis',(0.,0.,1.)) ;
#19112 = DIRECTION('',(0.,0.,-1.)) ;
#19113 = DIRECTION('',(0.,0.,-1.)) ;
#19114 = DIRECTION('center_axis',(0.,1.,0.)) ;
#19115 = DIRECTION('ref_axis',(-1.,0.,-1.22464679914735E-16)) ;
#19116 = DIRECTION('center_axis',(0.,-1.,0.)) ;
#19117 = DIRECTION('ref_axis',(1.,0.,0.)) ;
#19118 = DIRECTION('center_axis',(0.,1.,0.)) ;
#19119 = DIRECTION('ref_axis',(1.,0.,0.)) ;
#19120 = DIRECTION('center_axis',(0.,1.,0.)) ;
#19121 = DIRECTION('ref_axis',(-1.,0.,-5.66553889764798E-16)) ;
#19122 = DIRECTION('center_axis',(0.,-1.,0.)) ;
#19123 = DIRECTION('ref_axis',(1.,0.,0.)) ;
#19124 = DIRECTION('center_axis',(0.,1.,0.)) ;
#19125 = DIRECTION('ref_axis',(1.,0.,0.)) ;
#19126 = DIRECTION('center_axis',(0.,-1.,0.)) ;
#19127 = DIRECTION('ref_axis',(-1.,0.,0.)) ;
#19128 = DIRECTION('center_axis',(0.,1.,0.)) ;
#19129 = DIRECTION('ref_axis',(1.,0.,0.)) ;
#19130 = DIRECTION('',(0.,0.,1.)) ;
#19131 = DIRECTION('',(1.,0.,0.)) ;
#19132 = DIRECTION('',(0.,0.,1.)) ;
#19133 = DIRECTION('',(1.,0.,0.)) ;
#19134 = DIRECTION('',(0.,0.,1.)) ;
#19135 = DIRECTION('',(1.,0.,0.)) ;
#19136 = DIRECTION('',(0.,0.,1.)) ;
#19137 = DIRECTION('',(1.,0.,0.)) ;
#19138 = DIRECTION('',(0.,0.,1.)) ;
#19139 = DIRECTION('',(1.,0.,0.)) ;
#19140 = DIRECTION('',(0.,0.,1.)) ;
#19141 = DIRECTION('',(1.,0.,0.)) ;
#19142 = DIRECTION('',(0.,0.,1.)) ;
#19143 = DIRECTION('',(1.,0.,0.)) ;
#19144 = DIRECTION('',(0.,0.,1.)) ;
#19145 = DIRECTION('',(1.,0.,0.)) ;
#19146 = DIRECTION('',(0.,0.,1.)) ;
#19147 = DIRECTION('',(1.,0.,0.)) ;
#19148 = DIRECTION('',(0.,0.,1.)) ;
#19149 = DIRECTION('',(1.,0.,0.)) ;
#19150 = DIRECTION('',(0.,0.,1.)) ;
#19151 = DIRECTION('',(1.,0.,0.)) ;
#19152 = DIRECTION('',(0.,0.,1.)) ;
#19153 = DIRECTION('',(1.,0.,0.)) ;
#19154 = DIRECTION('axis',(0.,0.,1.)) ;
#19155 = DIRECTION('refdir',(1.,0.,0.)) ;
#19156 = DIRECTION('axis',(0.,0.,1.)) ;
#19157 = DIRECTION('refdir',(1.,0.,0.)) ;
#19158 = DIRECTION('center_axis',(0.,0.,1.)) ;
#19159 = DIRECTION('ref_axis',(1.,0.,0.)) ;
#19160 = DIRECTION('',(0.,0.,1.)) ;
#19161 = DIRECTION('center_axis',(1.,0.,0.)) ;
#19162 = DIRECTION('ref_axis',(0.,0.,-1.)) ;
#19163 = DIRECTION('center_axis',(1.,0.,0.)) ;
#19164 = DIRECTION('ref_axis',(0.,0.,-1.)) ;
#19165 = DIRECTION('',(1.,0.,0.)) ;
#19166 = DIRECTION('',(1.,0.,0.)) ;
#19167 = DIRECTION('center_axis',(-1.,0.,0.)) ;
#19168 = DIRECTION('ref_axis',(0.,0.,-1.)) ;
#19169 = DIRECTION('center_axis',(1.,0.,0.)) ;
#19170 = DIRECTION('ref_axis',(0.,0.,-1.)) ;
#19171 = DIRECTION('center_axis',(1.,0.,0.)) ;
#19172 = DIRECTION('ref_axis',(0.,0.,-1.)) ;
#19173 = DIRECTION('',(-1.,0.,0.)) ;
#19174 = DIRECTION('',(-1.,0.,0.)) ;
#19175 = DIRECTION('center_axis',(-1.,0.,0.)) ;
#19176 = DIRECTION('ref_axis',(0.,0.,-1.)) ;
#19177 = DIRECTION('center_axis',(-1.,0.,0.)) ;
#19178 = DIRECTION('ref_axis',(0.,0.,1.)) ;
#19179 = DIRECTION('center_axis',(1.,0.,0.)) ;
#19180 = DIRECTION('ref_axis',(0.,0.,-1.)) ;
#19181 = DIRECTION('axis',(0.,0.,1.)) ;
#19182 = DIRECTION('refdir',(1.,0.,0.)) ;
#19183 = DIRECTION('center_axis',(0.,0.,-1.)) ;
#19184 = DIRECTION('ref_axis',(-1.,0.,0.)) ;
#19185 = DIRECTION('',(-1.,0.,0.)) ;
#19186 = DIRECTION('center_axis',(0.,0.,-1.)) ;
#19187 = DIRECTION('ref_axis',(1.,0.,0.)) ;
#19188 = DIRECTION('',(1.,0.,0.)) ;
#19189 = DIRECTION('center_axis',(0.,0.,-1.)) ;
#19190 = DIRECTION('ref_axis',(1.,0.,0.)) ;
#19191 = DIRECTION('center_axis',(0.,0.,1.)) ;
#19192 = DIRECTION('ref_axis',(-1.,-1.22464679914735E-16,0.)) ;
#19193 = DIRECTION('center_axis',(0.,0.,-1.)) ;
#19194 = DIRECTION('ref_axis',(1.,0.,0.)) ;
#19195 = DIRECTION('center_axis',(0.,0.,1.)) ;
#19196 = DIRECTION('ref_axis',(1.,0.,0.)) ;
#19197 = DIRECTION('center_axis',(0.,0.,-1.)) ;
#19198 = DIRECTION('ref_axis',(1.,0.,0.)) ;
#19199 = DIRECTION('center_axis',(0.,0.,-1.)) ;
#19200 = DIRECTION('ref_axis',(-1.,0.,0.)) ;
#19201 = DIRECTION('',(1.,0.,0.)) ;
#19202 = DIRECTION('',(-1.,0.,0.)) ;
#19203 = DIRECTION('center_axis',(1.,0.,0.)) ;
#19204 = DIRECTION('ref_axis',(0.,0.,-1.)) ;
#19205 = DIRECTION('center_axis',(1.,0.,0.)) ;
#19206 = DIRECTION('ref_axis',(0.,0.,-1.)) ;
#19207 = DIRECTION('',(1.,0.,0.)) ;
#19208 = DIRECTION('',(1.,0.,0.)) ;
#19209 = DIRECTION('center_axis',(-1.,0.,0.)) ;
#19210 = DIRECTION('ref_axis',(0.,0.,-1.)) ;
#19211 = DIRECTION('center_axis',(1.,0.,0.)) ;
#19212 = DIRECTION('ref_axis',(0.,0.,-1.)) ;
#19213 = DIRECTION('center_axis',(1.,0.,0.)) ;
#19214 = DIRECTION('ref_axis',(0.,0.,-1.)) ;
#19215 = DIRECTION('',(-0.975609756097561,2.68824907129907E-17,-0.219512195121951)) ;
#19216 = DIRECTION('center_axis',(1.,0.,0.)) ;
#19217 = DIRECTION('ref_axis',(0.,0.,-1.)) ;
#19218 = DIRECTION('center_axis',(1.,0.,0.)) ;
#19219 = DIRECTION('ref_axis',(0.,0.,-1.)) ;
#19220 = DIRECTION('center_axis',(1.,0.,0.)) ;
#19221 = DIRECTION('ref_axis',(0.,0.,-1.)) ;
#19222 = DIRECTION('',(-1.,0.,0.)) ;
#19223 = DIRECTION('',(-1.,0.,0.)) ;
#19224 = DIRECTION('center_axis',(1.,0.,0.)) ;
#19225 = DIRECTION('ref_axis',(0.,0.,-1.)) ;
#19226 = DIRECTION('center_axis',(-1.,0.,0.)) ;
#19227 = DIRECTION('ref_axis',(0.,0.,-1.)) ;
#19228 = DIRECTION('',(-0.975609756097561,-2.68824907129907E-17,0.219512195121951)) ;
#19229 = DIRECTION('center_axis',(-1.,0.,0.)) ;
#19230 = DIRECTION('ref_axis',(0.,0.,-1.)) ;
#19231 = DIRECTION('center_axis',(-1.,0.,0.)) ;
#19232 = DIRECTION('ref_axis',(0.,0.,1.)) ;
#19233 = DIRECTION('axis',(0.,0.,1.)) ;
#19234 = DIRECTION('refdir',(1.,0.,0.)) ;
#19235 = DIRECTION('center_axis',(0.,0.,1.)) ;
#19236 = DIRECTION('ref_axis',(1.,0.,0.)) ;
#19237 = DIRECTION('center_axis',(0.,0.,1.)) ;
#19238 = DIRECTION('ref_axis',(1.,0.,0.)) ;
#19239 = DIRECTION('',(0.,0.,1.)) ;
#19240 = DIRECTION('center_axis',(0.,0.,-1.)) ;
#19241 = DIRECTION('ref_axis',(1.,0.,0.)) ;
#19242 = DIRECTION('center_axis',(0.,0.,1.)) ;
#19243 = DIRECTION('ref_axis',(1.,0.,0.)) ;
#19244 = DIRECTION('center_axis',(0.,0.,1.)) ;
#19245 = DIRECTION('ref_axis',(1.,0.,0.)) ;
#19246 = DIRECTION('',(0.,0.,-1.)) ;
#19247 = DIRECTION('center_axis',(0.,0.,-1.)) ;
#19248 = DIRECTION('ref_axis',(1.,0.,0.)) ;
#19249 = DIRECTION('center_axis',(0.,0.,-1.)) ;
#19250 = DIRECTION('ref_axis',(-1.,0.,0.)) ;
#19251 = DIRECTION('center_axis',(0.,0.,1.)) ;
#19252 = DIRECTION('ref_axis',(1.,0.,0.)) ;
#19253 = DIRECTION('axis',(0.,0.,1.)) ;
#19254 = DIRECTION('refdir',(1.,0.,0.)) ;
#19255 = DIRECTION('center_axis',(1.,0.,0.)) ;
#19256 = DIRECTION('ref_axis',(0.,0.,-1.)) ;
#19257 = DIRECTION('center_axis',(1.,0.,0.)) ;
#19258 = DIRECTION('ref_axis',(0.,0.,-1.)) ;
#19259 = DIRECTION('',(1.,0.,0.)) ;
#19260 = DIRECTION('center_axis',(-1.,0.,0.)) ;
#19261 = DIRECTION('ref_axis',(0.,0.,-1.)) ;
#19262 = DIRECTION('center_axis',(1.,0.,0.)) ;
#19263 = DIRECTION('ref_axis',(0.,0.,-1.)) ;
#19264 = DIRECTION('center_axis',(1.,0.,0.)) ;
#19265 = DIRECTION('ref_axis',(0.,0.,-1.)) ;
#19266 = DIRECTION('',(1.,0.,0.)) ;
#19267 = DIRECTION('center_axis',(-1.,0.,0.)) ;
#19268 = DIRECTION('ref_axis',(0.,0.,-1.)) ;
#19269 = DIRECTION('center_axis',(1.,0.,0.)) ;
#19270 = DIRECTION('ref_axis',(0.,0.,-1.)) ;
#19271 = DIRECTION('center_axis',(1.,0.,0.)) ;
#19272 = DIRECTION('ref_axis',(0.,0.,-1.)) ;
#19273 = DIRECTION('',(1.,0.,0.)) ;
#19274 = DIRECTION('center_axis',(-1.,0.,0.)) ;
#19275 = DIRECTION('ref_axis',(0.,0.,-1.)) ;
#19276 = DIRECTION('center_axis',(1.,0.,0.)) ;
#19277 = DIRECTION('ref_axis',(0.,0.,-1.)) ;
#19278 = DIRECTION('center_axis',(1.,0.,0.)) ;
#19279 = DIRECTION('ref_axis',(0.,0.,-1.)) ;
#19280 = DIRECTION('',(1.,0.,0.)) ;
#19281 = DIRECTION('center_axis',(-1.,0.,0.)) ;
#19282 = DIRECTION('ref_axis',(0.,0.,-1.)) ;
#19283 = DIRECTION('center_axis',(1.,0.,0.)) ;
#19284 = DIRECTION('ref_axis',(0.,0.,-1.)) ;
#19285 = DIRECTION('center_axis',(1.,0.,0.)) ;
#19286 = DIRECTION('ref_axis',(0.,0.,-1.)) ;
#19287 = DIRECTION('',(1.,0.,0.)) ;
#19288 = DIRECTION('center_axis',(-1.,0.,0.)) ;
#19289 = DIRECTION('ref_axis',(0.,0.,-1.)) ;
#19290 = DIRECTION('center_axis',(1.,0.,0.)) ;
#19291 = DIRECTION('ref_axis',(0.,0.,-1.)) ;
#19292 = DIRECTION('center_axis',(1.,0.,0.)) ;
#19293 = DIRECTION('ref_axis',(0.,0.,-1.)) ;
#19294 = DIRECTION('',(-1.,0.,0.)) ;
#19295 = DIRECTION('center_axis',(-1.,0.,0.)) ;
#19296 = DIRECTION('ref_axis',(0.,0.,-1.)) ;
#19297 = DIRECTION('center_axis',(-1.,0.,0.)) ;
#19298 = DIRECTION('ref_axis',(0.,0.,1.)) ;
#19299 = DIRECTION('center_axis',(1.,0.,0.)) ;
#19300 = DIRECTION('ref_axis',(0.,0.,-1.)) ;
#19301 = DIRECTION('axis',(0.,0.,1.)) ;
#19302 = DIRECTION('refdir',(1.,0.,0.)) ;
#19303 = DIRECTION('center_axis',(1.,0.,0.)) ;
#19304 = DIRECTION('ref_axis',(0.,0.,-1.)) ;
#19305 = DIRECTION('center_axis',(1.,0.,0.)) ;
#19306 = DIRECTION('ref_axis',(0.,0.,-1.)) ;
#19307 = DIRECTION('',(1.,0.,0.)) ;
#19308 = DIRECTION('center_axis',(-1.,0.,0.)) ;
#19309 = DIRECTION('ref_axis',(0.,0.,-1.)) ;
#19310 = DIRECTION('center_axis',(1.,0.,0.)) ;
#19311 = DIRECTION('ref_axis',(0.,0.,-1.)) ;
#19312 = DIRECTION('center_axis',(1.,0.,0.)) ;
#19313 = DIRECTION('ref_axis',(0.,0.,-1.)) ;
#19314 = DIRECTION('',(1.,0.,0.)) ;
#19315 = DIRECTION('center_axis',(-1.,0.,0.)) ;
#19316 = DIRECTION('ref_axis',(0.,0.,-1.)) ;
#19317 = DIRECTION('center_axis',(1.,0.,0.)) ;
#19318 = DIRECTION('ref_axis',(0.,0.,-1.)) ;
#19319 = DIRECTION('center_axis',(1.,0.,0.)) ;
#19320 = DIRECTION('ref_axis',(0.,0.,-1.)) ;
#19321 = DIRECTION('',(1.,0.,0.)) ;
#19322 = DIRECTION('center_axis',(-1.,0.,0.)) ;
#19323 = DIRECTION('ref_axis',(0.,0.,-1.)) ;
#19324 = DIRECTION('center_axis',(1.,0.,0.)) ;
#19325 = DIRECTION('ref_axis',(0.,0.,-1.)) ;
#19326 = DIRECTION('center_axis',(1.,0.,0.)) ;
#19327 = DIRECTION('ref_axis',(0.,0.,-1.)) ;
#19328 = DIRECTION('',(1.,0.,0.)) ;
#19329 = DIRECTION('center_axis',(-1.,0.,0.)) ;
#19330 = DIRECTION('ref_axis',(0.,0.,-1.)) ;
#19331 = DIRECTION('center_axis',(1.,0.,0.)) ;
#19332 = DIRECTION('ref_axis',(0.,0.,-1.)) ;
#19333 = DIRECTION('center_axis',(1.,0.,0.)) ;
#19334 = DIRECTION('ref_axis',(0.,0.,-1.)) ;
#19335 = DIRECTION('',(1.,0.,0.)) ;
#19336 = DIRECTION('center_axis',(-1.,0.,0.)) ;
#19337 = DIRECTION('ref_axis',(0.,0.,-1.)) ;
#19338 = DIRECTION('center_axis',(1.,0.,0.)) ;
#19339 = DIRECTION('ref_axis',(0.,0.,-1.)) ;
#19340 = DIRECTION('center_axis',(1.,0.,0.)) ;
#19341 = DIRECTION('ref_axis',(0.,0.,-1.)) ;
#19342 = DIRECTION('',(-1.,0.,0.)) ;
#19343 = DIRECTION('center_axis',(-1.,0.,0.)) ;
#19344 = DIRECTION('ref_axis',(0.,0.,-1.)) ;
#19345 = DIRECTION('center_axis',(-1.,0.,0.)) ;
#19346 = DIRECTION('ref_axis',(0.,0.,1.)) ;
#19347 = DIRECTION('center_axis',(1.,0.,0.)) ;
#19348 = DIRECTION('ref_axis',(0.,0.,-1.)) ;
#19349 = DIRECTION('axis',(0.,0.,1.)) ;
#19350 = DIRECTION('refdir',(1.,0.,0.)) ;
#19351 = DIRECTION('center_axis',(0.,0.,1.)) ;
#19352 = DIRECTION('ref_axis',(1.,0.,0.)) ;
#19353 = DIRECTION('',(-1.,0.,0.)) ;
#19354 = DIRECTION('center_axis',(0.,0.,1.)) ;
#19355 = DIRECTION('ref_axis',(1.,0.,0.)) ;
#19356 = DIRECTION('center_axis',(0.,0.,1.)) ;
#19357 = DIRECTION('ref_axis',(1.,0.,0.)) ;
#19358 = DIRECTION('center_axis',(0.,0.,1.)) ;
#19359 = DIRECTION('ref_axis',(1.,0.,0.)) ;
#19360 = DIRECTION('',(0.,0.,1.)) ;
#19361 = DIRECTION('center_axis',(0.,0.,-1.)) ;
#19362 = DIRECTION('ref_axis',(1.,0.,0.)) ;
#19363 = DIRECTION('center_axis',(0.,0.,1.)) ;
#19364 = DIRECTION('ref_axis',(1.,0.,0.)) ;
#19365 = DIRECTION('center_axis',(0.,0.,1.)) ;
#19366 = DIRECTION('ref_axis',(1.,0.,0.)) ;
#19367 = DIRECTION('',(1.,0.,0.)) ;
#19368 = DIRECTION('center_axis',(0.,0.,1.)) ;
#19369 = DIRECTION('ref_axis',(1.,0.,0.)) ;
#19370 = DIRECTION('center_axis',(0.,0.,1.)) ;
#19371 = DIRECTION('ref_axis',(1.,0.,0.)) ;
#19372 = DIRECTION('center_axis',(0.,0.,1.)) ;
#19373 = DIRECTION('ref_axis',(1.,0.,0.)) ;
#19374 = DIRECTION('',(0.,0.,1.)) ;
#19375 = DIRECTION('center_axis',(0.,0.,-1.)) ;
#19376 = DIRECTION('ref_axis',(1.,0.,0.)) ;
#19377 = DIRECTION('center_axis',(0.,0.,1.)) ;
#19378 = DIRECTION('ref_axis',(1.,0.,0.)) ;
#19379 = DIRECTION('center_axis',(0.,0.,1.)) ;
#19380 = DIRECTION('ref_axis',(1.,0.,0.)) ;
#19381 = DIRECTION('',(1.,0.,0.)) ;
#19382 = DIRECTION('',(0.,-1.,0.)) ;
#19383 = DIRECTION('',(1.,0.,0.)) ;
#19384 = DIRECTION('',(0.,1.,0.)) ;
#19385 = DIRECTION('center_axis',(0.,0.,1.)) ;
#19386 = DIRECTION('ref_axis',(1.,0.,0.)) ;
#19387 = DIRECTION('',(-1.,0.,0.)) ;
#19388 = DIRECTION('',(0.,1.,0.)) ;
#19389 = DIRECTION('',(-1.,0.,0.)) ;
#19390 = DIRECTION('',(0.,-1.,0.)) ;
#19391 = DIRECTION('center_axis',(0.,0.,1.)) ;
#19392 = DIRECTION('ref_axis',(1.,0.,0.)) ;
#19393 = DIRECTION('',(0.,-1.,0.)) ;
#19394 = DIRECTION('',(-1.,0.,0.)) ;
#19395 = DIRECTION('',(0.,1.,0.)) ;
#19396 = DIRECTION('',(1.,0.,0.)) ;
#19397 = DIRECTION('center_axis',(0.,1.,0.)) ;
#19398 = DIRECTION('ref_axis',(0.,0.,1.)) ;
#19399 = DIRECTION('',(0.,0.,-1.)) ;
#19400 = DIRECTION('',(0.,0.,-1.)) ;
#19401 = DIRECTION('center_axis',(0.,-1.,0.)) ;
#19402 = DIRECTION('ref_axis',(0.,0.,-1.)) ;
#19403 = DIRECTION('',(0.,0.,-1.)) ;
#19404 = DIRECTION('',(0.,0.,-1.)) ;
#19405 = DIRECTION('center_axis',(-1.,0.,0.)) ;
#19406 = DIRECTION('ref_axis',(0.,0.,1.)) ;
#19407 = DIRECTION('center_axis',(-1.,0.,0.)) ;
#19408 = DIRECTION('ref_axis',(0.,0.,-1.)) ;
#19409 = DIRECTION('center_axis',(1.,0.,0.)) ;
#19410 = DIRECTION('ref_axis',(0.,0.,-1.)) ;
#19411 = DIRECTION('center_axis',(1.,0.,0.)) ;
#19412 = DIRECTION('ref_axis',(0.,1.22464679914735E-16,1.)) ;
#19413 = DIRECTION('center_axis',(1.,0.,0.)) ;
#19414 = DIRECTION('ref_axis',(0.,0.,-1.)) ;
#19415 = DIRECTION('center_axis',(1.,0.,0.)) ;
#19416 = DIRECTION('ref_axis',(0.,0.,-1.)) ;
#19417 = DIRECTION('',(1.,0.,0.)) ;
#19418 = DIRECTION('center_axis',(-1.,0.,0.)) ;
#19419 = DIRECTION('ref_axis',(0.,0.,-1.)) ;
#19420 = DIRECTION('center_axis',(1.,0.,0.)) ;
#19421 = DIRECTION('ref_axis',(0.,0.,-1.)) ;
#19422 = DIRECTION('',(0.,0.,1.)) ;
#19423 = DIRECTION('',(1.,0.,0.)) ;
#19424 = DIRECTION('',(0.,0.,1.)) ;
#19425 = DIRECTION('',(1.,0.,0.)) ;
#19426 = DIRECTION('',(0.,0.,1.)) ;
#19427 = DIRECTION('',(1.,0.,0.)) ;
#19428 = DIRECTION('',(0.,0.,1.)) ;
#19429 = DIRECTION('',(1.,0.,0.)) ;
#19430 = DIRECTION('',(0.,0.,1.)) ;
#19431 = DIRECTION('',(1.,0.,0.)) ;
#19432 = DIRECTION('',(0.,0.,1.)) ;
#19433 = DIRECTION('',(1.,0.,0.)) ;
#19434 = DIRECTION('',(0.,0.,1.)) ;
#19435 = DIRECTION('',(1.,0.,0.)) ;
#19436 = DIRECTION('axis',(0.,0.,1.)) ;
#19437 = DIRECTION('refdir',(1.,0.,0.)) ;
#19438 = DIRECTION('axis',(0.,0.,1.)) ;
#19439 = DIRECTION('refdir',(1.,0.,0.)) ;
#19440 = DIRECTION('center_axis',(0.,-1.,0.)) ;
#19441 = DIRECTION('ref_axis',(1.,0.,0.)) ;
#19442 = DIRECTION('center_axis',(0.,-1.,0.)) ;
#19443 = DIRECTION('ref_axis',(1.,0.,0.)) ;
#19444 = DIRECTION('',(0.,1.,0.)) ;
#19445 = DIRECTION('center_axis',(0.,1.,0.)) ;
#19446 = DIRECTION('ref_axis',(1.,0.,0.)) ;
#19447 = DIRECTION('center_axis',(0.,-1.,0.)) ;
#19448 = DIRECTION('ref_axis',(1.,0.,0.)) ;
#19449 = DIRECTION('center_axis',(0.,-1.,0.)) ;
#19450 = DIRECTION('ref_axis',(1.,0.,0.)) ;
#19451 = DIRECTION('center_axis',(0.,-1.,0.)) ;
#19452 = DIRECTION('ref_axis',(1.,0.,0.)) ;
#19453 = DIRECTION('',(0.,1.,0.)) ;
#19454 = DIRECTION('center_axis',(0.,1.,0.)) ;
#19455 = DIRECTION('ref_axis',(1.,0.,0.)) ;
#19456 = DIRECTION('center_axis',(0.,1.,0.)) ;
#19457 = DIRECTION('ref_axis',(-1.,0.,0.)) ;
#19458 = DIRECTION('center_axis',(0.,-1.,0.)) ;
#19459 = DIRECTION('ref_axis',(1.,0.,0.)) ;
#19460 = DIRECTION('axis',(0.,0.,1.)) ;
#19461 = DIRECTION('refdir',(1.,0.,0.)) ;
#19462 = DIRECTION('center_axis',(0.,1.,0.)) ;
#19463 = DIRECTION('ref_axis',(1.,0.,0.)) ;
#19464 = DIRECTION('center_axis',(0.,1.,0.)) ;
#19465 = DIRECTION('ref_axis',(1.,0.,0.)) ;
#19466 = DIRECTION('',(0.,1.,0.)) ;
#19467 = DIRECTION('center_axis',(0.,-1.,0.)) ;
#19468 = DIRECTION('ref_axis',(1.,0.,0.)) ;
#19469 = DIRECTION('center_axis',(0.,1.,0.)) ;
#19470 = DIRECTION('ref_axis',(1.,0.,0.)) ;
#19471 = DIRECTION('center_axis',(0.,1.,0.)) ;
#19472 = DIRECTION('ref_axis',(1.,0.,0.)) ;
#19473 = DIRECTION('',(0.,-1.,0.)) ;
#19474 = DIRECTION('center_axis',(0.,-1.,0.)) ;
#19475 = DIRECTION('ref_axis',(1.,0.,0.)) ;
#19476 = DIRECTION('center_axis',(0.,-1.,0.)) ;
#19477 = DIRECTION('ref_axis',(-1.,0.,0.)) ;
#19478 = DIRECTION('center_axis',(0.,1.,0.)) ;
#19479 = DIRECTION('ref_axis',(1.,0.,0.)) ;
#19480 = DIRECTION('axis',(0.,0.,1.)) ;
#19481 = DIRECTION('refdir',(1.,0.,0.)) ;
#19482 = DIRECTION('center_axis',(0.,1.,0.)) ;
#19483 = DIRECTION('ref_axis',(1.,0.,0.)) ;
#19484 = DIRECTION('center_axis',(0.,1.,0.)) ;
#19485 = DIRECTION('ref_axis',(1.,0.,0.)) ;
#19486 = DIRECTION('',(0.,1.,0.)) ;
#19487 = DIRECTION('center_axis',(0.,-1.,0.)) ;
#19488 = DIRECTION('ref_axis',(1.,0.,0.)) ;
#19489 = DIRECTION('center_axis',(-0.5,0.,-0.866025403784439)) ;
#19490 = DIRECTION('ref_axis',(-0.866025403784439,0.,0.5)) ;
#19491 = DIRECTION('',(0.,1.,0.)) ;
#19492 = DIRECTION('',(0.866025403784439,0.,-0.5)) ;
#19493 = DIRECTION('',(0.,-1.,0.)) ;
#19494 = DIRECTION('',(-0.866025403784439,0.,0.5)) ;
#19495 = DIRECTION('center_axis',(0.5,0.,0.866025403784439)) ;
#19496 = DIRECTION('ref_axis',(0.866025403784439,0.,-0.5)) ;
#19497 = DIRECTION('',(0.,1.,0.)) ;
#19498 = DIRECTION('',(-0.866025403784439,0.,0.5)) ;
#19499 = DIRECTION('',(0.,-1.,0.)) ;
#19500 = DIRECTION('',(0.866025403784439,0.,-0.5)) ;
#19501 = DIRECTION('center_axis',(0.,-1.,0.)) ;
#19502 = DIRECTION('ref_axis',(-1.,0.,0.)) ;
#19503 = DIRECTION('',(0.866025403784439,0.,0.5)) ;
#19504 = DIRECTION('',(0.,0.,1.)) ;
#19505 = DIRECTION('',(-0.866025403784439,0.,-0.5)) ;
#19506 = DIRECTION('',(0.,0.,-1.)) ;
#19507 = DIRECTION('center_axis',(0.5,0.,-0.866025403784439)) ;
#19508 = DIRECTION('ref_axis',(-0.866025403784439,0.,-0.5)) ;
#19509 = DIRECTION('',(0.,1.,0.)) ;
#19510 = DIRECTION('',(-0.866025403784439,0.,-0.5)) ;
#19511 = DIRECTION('center_axis',(-0.5,0.,0.866025403784439)) ;
#19512 = DIRECTION('ref_axis',(0.866025403784439,0.,0.5)) ;
#19513 = DIRECTION('',(0.,1.,0.)) ;
#19514 = DIRECTION('',(0.866025403784439,0.,0.5)) ;
#19515 = DIRECTION('center_axis',(1.,0.,0.)) ;
#19516 = DIRECTION('ref_axis',(0.,0.,-1.)) ;
#19517 = DIRECTION('',(0.,0.,-1.)) ;
#19518 = DIRECTION('center_axis',(-1.,0.,0.)) ;
#19519 = DIRECTION('ref_axis',(0.,0.,1.)) ;
#19520 = DIRECTION('',(0.,0.,1.)) ;
#19521 = DIRECTION('center_axis',(0.,1.,0.)) ;
#19522 = DIRECTION('ref_axis',(1.,0.,0.)) ;
#19523 = DIRECTION('axis',(0.,0.,1.)) ;
#19524 = DIRECTION('refdir',(1.,0.,0.)) ;
#19525 = DIRECTION('center_axis',(0.,1.,0.)) ;
#19526 = DIRECTION('ref_axis',(1.,0.,0.)) ;
#19527 = DIRECTION('center_axis',(0.,1.,0.)) ;
#19528 = DIRECTION('ref_axis',(1.,0.,0.)) ;
#19529 = DIRECTION('',(0.,-1.,0.)) ;
#19530 = DIRECTION('center_axis',(0.,-1.,0.)) ;
#19531 = DIRECTION('ref_axis',(1.,0.,0.)) ;
#19532 = DIRECTION('center_axis',(0.,1.,0.)) ;
#19533 = DIRECTION('ref_axis',(1.,0.,0.)) ;
#19534 = DIRECTION('center_axis',(-0.5,0.,-0.866025403784439)) ;
#19535 = DIRECTION('ref_axis',(-0.866025403784439,0.,0.5)) ;
#19536 = DIRECTION('',(0.,1.,0.)) ;
#19537 = DIRECTION('',(0.866025403784439,0.,-0.5)) ;
#19538 = DIRECTION('',(0.,-1.,0.)) ;
#19539 = DIRECTION('',(-0.866025403784439,0.,0.5)) ;
#19540 = DIRECTION('center_axis',(0.5,0.,0.866025403784439)) ;
#19541 = DIRECTION('ref_axis',(0.866025403784439,0.,-0.5)) ;
#19542 = DIRECTION('',(0.,1.,0.)) ;
#19543 = DIRECTION('',(-0.866025403784439,0.,0.5)) ;
#19544 = DIRECTION('',(0.,-1.,0.)) ;
#19545 = DIRECTION('',(0.866025403784439,0.,-0.5)) ;
#19546 = DIRECTION('center_axis',(0.,-1.,0.)) ;
#19547 = DIRECTION('ref_axis',(-1.,0.,0.)) ;
#19548 = DIRECTION('',(0.866025403784439,0.,0.5)) ;
#19549 = DIRECTION('',(0.,0.,1.)) ;
#19550 = DIRECTION('',(-0.866025403784439,0.,-0.5)) ;
#19551 = DIRECTION('',(0.,0.,-1.)) ;
#19552 = DIRECTION('center_axis',(0.5,0.,-0.866025403784439)) ;
#19553 = DIRECTION('ref_axis',(-0.866025403784439,0.,-0.5)) ;
#19554 = DIRECTION('',(0.,1.,0.)) ;
#19555 = DIRECTION('',(-0.866025403784439,0.,-0.5)) ;
#19556 = DIRECTION('center_axis',(-0.5,0.,0.866025403784439)) ;
#19557 = DIRECTION('ref_axis',(0.866025403784439,0.,0.5)) ;
#19558 = DIRECTION('',(0.,1.,0.)) ;
#19559 = DIRECTION('',(0.866025403784439,0.,0.5)) ;
#19560 = DIRECTION('center_axis',(1.,0.,0.)) ;
#19561 = DIRECTION('ref_axis',(0.,0.,-1.)) ;
#19562 = DIRECTION('',(0.,0.,-1.)) ;
#19563 = DIRECTION('center_axis',(-1.,0.,0.)) ;
#19564 = DIRECTION('ref_axis',(0.,0.,1.)) ;
#19565 = DIRECTION('',(0.,0.,1.)) ;
#19566 = DIRECTION('center_axis',(0.,1.,0.)) ;
#19567 = DIRECTION('ref_axis',(1.,0.,0.)) ;
#19568 = DIRECTION('axis',(0.,0.,1.)) ;
#19569 = DIRECTION('refdir',(1.,0.,0.)) ;
#19570 = DIRECTION('center_axis',(0.,-1.,0.)) ;
#19571 = DIRECTION('ref_axis',(1.,0.,0.)) ;
#19572 = DIRECTION('center_axis',(0.,-1.,0.)) ;
#19573 = DIRECTION('ref_axis',(1.,0.,0.)) ;
#19574 = DIRECTION('',(0.,1.,0.)) ;
#19575 = DIRECTION('center_axis',(0.,1.,0.)) ;
#19576 = DIRECTION('ref_axis',(1.,0.,0.)) ;
#19577 = DIRECTION('center_axis',(0.,-1.,0.)) ;
#19578 = DIRECTION('ref_axis',(1.,0.,0.)) ;
#19579 = DIRECTION('center_axis',(-0.5,0.,0.866025403784439)) ;
#19580 = DIRECTION('ref_axis',(-0.866025403784439,0.,-0.5)) ;
#19581 = DIRECTION('',(0.,-1.,0.)) ;
#19582 = DIRECTION('',(0.866025403784439,0.,0.5)) ;
#19583 = DIRECTION('',(0.,1.,0.)) ;
#19584 = DIRECTION('',(-0.866025403784439,0.,-0.5)) ;
#19585 = DIRECTION('center_axis',(0.5,0.,-0.866025403784439)) ;
#19586 = DIRECTION('ref_axis',(0.866025403784439,0.,0.5)) ;
#19587 = DIRECTION('',(0.,-1.,0.)) ;
#19588 = DIRECTION('',(-0.866025403784439,0.,-0.5)) ;
#19589 = DIRECTION('',(0.,1.,0.)) ;
#19590 = DIRECTION('',(0.866025403784439,0.,0.5)) ;
#19591 = DIRECTION('center_axis',(0.,1.,0.)) ;
#19592 = DIRECTION('ref_axis',(-1.,0.,0.)) ;
#19593 = DIRECTION('',(0.866025403784439,0.,-0.5)) ;
#19594 = DIRECTION('',(0.,0.,-1.)) ;
#19595 = DIRECTION('',(-0.866025403784439,0.,0.5)) ;
#19596 = DIRECTION('',(0.,0.,1.)) ;
#19597 = DIRECTION('center_axis',(0.5,0.,0.866025403784439)) ;
#19598 = DIRECTION('ref_axis',(-0.866025403784439,0.,0.5)) ;
#19599 = DIRECTION('',(0.,-1.,0.)) ;
#19600 = DIRECTION('',(-0.866025403784439,0.,0.5)) ;
#19601 = DIRECTION('center_axis',(-0.5,0.,-0.866025403784439)) ;
#19602 = DIRECTION('ref_axis',(0.866025403784439,0.,-0.5)) ;
#19603 = DIRECTION('',(0.,-1.,0.)) ;
#19604 = DIRECTION('',(0.866025403784439,0.,-0.5)) ;
#19605 = DIRECTION('center_axis',(1.,0.,0.)) ;
#19606 = DIRECTION('ref_axis',(0.,0.,1.)) ;
#19607 = DIRECTION('',(0.,0.,1.)) ;
#19608 = DIRECTION('center_axis',(-1.,0.,0.)) ;
#19609 = DIRECTION('ref_axis',(0.,0.,-1.)) ;
#19610 = DIRECTION('',(0.,0.,-1.)) ;
#19611 = DIRECTION('center_axis',(0.,-1.,0.)) ;
#19612 = DIRECTION('ref_axis',(1.,0.,0.)) ;
#19613 = DIRECTION('axis',(0.,0.,1.)) ;
#19614 = DIRECTION('refdir',(1.,0.,0.)) ;
#19615 = DIRECTION('center_axis',(0.,1.,0.)) ;
#19616 = DIRECTION('ref_axis',(1.,0.,0.)) ;
#19617 = DIRECTION('center_axis',(0.,1.,0.)) ;
#19618 = DIRECTION('ref_axis',(1.,0.,0.)) ;
#19619 = DIRECTION('',(0.,1.,0.)) ;
#19620 = DIRECTION('center_axis',(0.,-1.,0.)) ;
#19621 = DIRECTION('ref_axis',(1.,0.,0.)) ;
#19622 = DIRECTION('center_axis',(-0.5,0.,-0.866025403784439)) ;
#19623 = DIRECTION('ref_axis',(-0.866025403784439,0.,0.5)) ;
#19624 = DIRECTION('',(0.,1.,0.)) ;
#19625 = DIRECTION('',(0.866025403784439,0.,-0.5)) ;
#19626 = DIRECTION('',(0.,-1.,0.)) ;
#19627 = DIRECTION('',(-0.866025403784439,0.,0.5)) ;
#19628 = DIRECTION('center_axis',(0.5,0.,0.866025403784439)) ;
#19629 = DIRECTION('ref_axis',(0.866025403784439,0.,-0.5)) ;
#19630 = DIRECTION('',(0.,1.,0.)) ;
#19631 = DIRECTION('',(-0.866025403784439,0.,0.5)) ;
#19632 = DIRECTION('',(0.,-1.,0.)) ;
#19633 = DIRECTION('',(0.866025403784439,0.,-0.5)) ;
#19634 = DIRECTION('center_axis',(0.,-1.,0.)) ;
#19635 = DIRECTION('ref_axis',(-1.,0.,0.)) ;
#19636 = DIRECTION('',(0.866025403784439,0.,0.5)) ;
#19637 = DIRECTION('',(0.,0.,1.)) ;
#19638 = DIRECTION('',(-0.866025403784439,0.,-0.5)) ;
#19639 = DIRECTION('',(0.,0.,-1.)) ;
#19640 = DIRECTION('center_axis',(0.5,0.,-0.866025403784439)) ;
#19641 = DIRECTION('ref_axis',(-0.866025403784439,0.,-0.5)) ;
#19642 = DIRECTION('',(0.,1.,0.)) ;
#19643 = DIRECTION('',(-0.866025403784439,0.,-0.5)) ;
#19644 = DIRECTION('center_axis',(-0.5,0.,0.866025403784439)) ;
#19645 = DIRECTION('ref_axis',(0.866025403784439,0.,0.5)) ;
#19646 = DIRECTION('',(0.,1.,0.)) ;
#19647 = DIRECTION('',(0.866025403784439,0.,0.5)) ;
#19648 = DIRECTION('center_axis',(1.,0.,0.)) ;
#19649 = DIRECTION('ref_axis',(0.,0.,-1.)) ;
#19650 = DIRECTION('',(0.,0.,-1.)) ;
#19651 = DIRECTION('center_axis',(-1.,0.,0.)) ;
#19652 = DIRECTION('ref_axis',(0.,0.,1.)) ;
#19653 = DIRECTION('',(0.,0.,1.)) ;
#19654 = DIRECTION('center_axis',(0.,1.,0.)) ;
#19655 = DIRECTION('ref_axis',(1.,0.,0.)) ;
#19656 = DIRECTION('',(0.,0.,1.)) ;
#19657 = DIRECTION('',(1.,0.,0.)) ;
#19658 = DIRECTION('',(0.,0.,1.)) ;
#19659 = DIRECTION('',(1.,0.,0.)) ;
#19660 = DIRECTION('',(0.,0.,1.)) ;
#19661 = DIRECTION('',(1.,0.,0.)) ;
#19662 = DIRECTION('',(0.,0.,1.)) ;
#19663 = DIRECTION('',(1.,0.,0.)) ;
#19664 = DIRECTION('',(0.,0.,1.)) ;
#19665 = DIRECTION('',(1.,0.,0.)) ;
#19666 = DIRECTION('',(0.,0.,1.)) ;
#19667 = DIRECTION('',(1.,0.,0.)) ;
#19668 = DIRECTION('',(0.,0.,1.)) ;
#19669 = DIRECTION('',(1.,0.,0.)) ;
#19670 = DIRECTION('',(0.,0.,1.)) ;
#19671 = DIRECTION('',(1.,0.,0.)) ;
#19672 = DIRECTION('',(0.,0.,1.)) ;
#19673 = DIRECTION('',(1.,0.,0.)) ;
#19674 = DIRECTION('',(0.,0.,1.)) ;
#19675 = DIRECTION('',(1.,0.,0.)) ;
#19676 = DIRECTION('',(0.,0.,1.)) ;
#19677 = DIRECTION('',(1.,0.,0.)) ;
#19678 = DIRECTION('',(0.,0.,1.)) ;
#19679 = DIRECTION('',(1.,0.,0.)) ;
#19680 = DIRECTION('',(0.,0.,1.)) ;
#19681 = DIRECTION('',(1.,0.,0.)) ;
#19682 = DIRECTION('',(0.,0.,1.)) ;
#19683 = DIRECTION('',(1.,0.,0.)) ;
#19684 = DIRECTION('',(0.,0.,1.)) ;
#19685 = DIRECTION('',(1.,0.,0.)) ;
#19686 = DIRECTION('',(0.,0.,1.)) ;
#19687 = DIRECTION('',(1.,0.,0.)) ;
#19688 = DIRECTION('',(0.,0.,1.)) ;
#19689 = DIRECTION('',(1.,0.,0.)) ;
#19690 = DIRECTION('',(0.,0.,1.)) ;
#19691 = DIRECTION('',(1.,0.,0.)) ;
#19692 = DIRECTION('',(0.,0.,1.)) ;
#19693 = DIRECTION('',(1.,0.,0.)) ;
#19694 = DIRECTION('',(0.,0.,1.)) ;
#19695 = DIRECTION('',(1.,0.,0.)) ;
#19696 = DIRECTION('',(0.,0.,1.)) ;
#19697 = DIRECTION('',(1.,0.,0.)) ;
#19698 = DIRECTION('',(0.,0.,1.)) ;
#19699 = DIRECTION('',(1.,0.,0.)) ;
#19700 = DIRECTION('',(0.,0.,1.)) ;
#19701 = DIRECTION('',(1.,0.,0.)) ;
#19702 = CARTESIAN_POINT('',(0.,0.,0.)) ;
#19703 = CARTESIAN_POINT('',(0.,0.,0.)) ;
#19704 = CARTESIAN_POINT('',(0.,0.,0.)) ;
#19705 = CARTESIAN_POINT('Origin',(2.5,-3.5,11.5)) ;
#19706 = CARTESIAN_POINT('',(2.59406867944788,-3.5,11.1009372435983)) ;
#19707 = CARTESIAN_POINT('',(2.24874539997451,-3.5,11.1760075217447)) ;
#19708 = CARTESIAN_POINT('Origin',(0.,-3.5,0.)) ;
#19709 = CARTESIAN_POINT('',(2.09,-3.5,11.5)) ;
#19710 = CARTESIAN_POINT('Origin',(2.5,-3.5,11.5)) ;
#19711 = CARTESIAN_POINT('Origin',(2.5,-3.5,11.5)) ;
#19712 = CARTESIAN_POINT('Origin',(2.5,-4.1,11.5)) ;
#19713 = CARTESIAN_POINT('',(2.09,-4.6,11.5)) ;
#19714 = CARTESIAN_POINT('Origin',(2.5,-4.6,11.5)) ;
#19715 = CARTESIAN_POINT('',(2.09,-4.1,11.5)) ;
#19716 = CARTESIAN_POINT('',(2.59406867944801,-3.6,11.1009372435983)) ;
#19717 = CARTESIAN_POINT('',(2.59406867944788,-4.1,11.1009372435983)) ;
#19718 = CARTESIAN_POINT('',(2.24874539997437,-3.6,11.1760075217447)) ;
#19719 = CARTESIAN_POINT('Origin',(2.5,-3.6,11.5)) ;
#19720 = CARTESIAN_POINT('',(2.24874539997451,-4.1,11.1760075217447)) ;
#19721 = CARTESIAN_POINT('Origin',(0.,-1.8,0.)) ;
#19722 = CARTESIAN_POINT('',(-2.24874539997437,-3.6,11.1760075217447)) ;
#19723 = CARTESIAN_POINT('Origin',(0.,-3.6,0.)) ;
#19724 = CARTESIAN_POINT('',(-2.24874539997451,-3.5,11.1760075217447)) ;
#19725 = CARTESIAN_POINT('',(-2.24874539997451,-4.1,11.1760075217447)) ;
#19726 = CARTESIAN_POINT('',(-2.59406867944788,-3.5,11.1009372435983)) ;
#19727 = CARTESIAN_POINT('Origin',(0.,-3.5,0.)) ;
#19728 = CARTESIAN_POINT('',(-2.59406867944801,-3.6,11.1009372435983)) ;
#19729 = CARTESIAN_POINT('',(-2.59406867944788,-4.1,11.1009372435983)) ;
#19730 = CARTESIAN_POINT('',(-11.4,-3.6,1.39609735102798E-15)) ;
#19731 = CARTESIAN_POINT('Origin',(0.,-3.6,0.)) ;
#19732 = CARTESIAN_POINT('',(-11.4,-0.0999999999999999,-1.39609735102798E-15)) ;
#19733 = CARTESIAN_POINT('',(-11.4,-1.8,1.39609735102798E-15)) ;
#19734 = CARTESIAN_POINT('Origin',(0.,-0.0999999999999999,0.)) ;
#19735 = CARTESIAN_POINT('',(7.40055690846941,-3.6,-8.67131809153059)) ;
#19736 = CARTESIAN_POINT('Origin',(0.,-3.6,0.)) ;
#19737 = CARTESIAN_POINT('',(7.40055690846942,-3.,-8.67131809153058)) ;
#19738 = CARTESIAN_POINT('',(7.40055690846942,-4.65,-8.67131809153058)) ;
#19739 = CARTESIAN_POINT('',(8.67131809153058,-3.,-7.40055690846942)) ;
#19740 = CARTESIAN_POINT('Origin',(0.,-3.,0.)) ;
#19741 = CARTESIAN_POINT('',(8.67131809153059,-3.6,-7.40055690846941)) ;
#19742 = CARTESIAN_POINT('',(8.67131809153058,-4.65,-7.40055690846942)) ;
#19743 = CARTESIAN_POINT('Origin',(0.,-3.6,0.)) ;
#19744 = CARTESIAN_POINT('',(-2.12602916254692,-2.46796330384352,-11.2)) ;
#19745 = CARTESIAN_POINT('',(-4.1,-1.8,-10.6371988794043)) ;
#19746 = CARTESIAN_POINT('Ctrl Pts',(-2.12602916254691,-2.46796330384352,
-11.2)) ;
#19747 = CARTESIAN_POINT('Ctrl Pts',(-2.15513164480001,-2.50604132495688,
-11.1944756494667)) ;
#19748 = CARTESIAN_POINT('Ctrl Pts',(-2.18630985484209,-2.54164208401901,
-11.1884379436503)) ;
#19749 = CARTESIAN_POINT('Ctrl Pts',(-2.31779618826562,-2.67429360771505,
-11.1623481119451)) ;
#19750 = CARTESIAN_POINT('Ctrl Pts',(-2.44303520251314,-2.75997478721919,
-11.1360298274263)) ;
#19751 = CARTESIAN_POINT('Ctrl Pts',(-2.71564409591941,-2.87280151063408,
-11.0727078200836)) ;
#19752 = CARTESIAN_POINT('Ctrl Pts',(-2.86295917531106,-2.9,-11.0355626174438)) ;
#19753 = CARTESIAN_POINT('Ctrl Pts',(-3.13999995839577,-2.9,-10.9599935484512)) ;
#19754 = CARTESIAN_POINT('Ctrl Pts',(-3.28870394625325,-2.87173395468652,
-10.9162703933172)) ;
#19755 = CARTESIAN_POINT('Ctrl Pts',(-3.5620474526488,-2.75711351549606,-10.8301593198666)) ;
#19756 = CARTESIAN_POINT('Ctrl Pts',(-3.68673548477559,-2.67077361394648,
-10.787906168642)) ;
#19757 = CARTESIAN_POINT('Ctrl Pts',(-3.87930809485592,-2.47439729417,-10.7201158159833)) ;
#19758 = CARTESIAN_POINT('Ctrl Pts',(-3.96197425311411,-2.35282868058528,
-10.6895386999817)) ;
#19759 = CARTESIAN_POINT('Ctrl Pts',(-4.07235177185144,-2.08473780880403,
-10.6479776813726)) ;
#19760 = CARTESIAN_POINT('Ctrl Pts',(-4.1,-1.93815780811578,-10.6371988794043)) ;
#19761 = CARTESIAN_POINT('Ctrl Pts',(-4.1,-1.8,-10.6371988794043)) ;
#19762 = CARTESIAN_POINT('',(-2.12602916254692,-1.13203669615648,-11.2)) ;
#19763 = CARTESIAN_POINT('Ctrl Pts',(-4.1,-1.8,-10.6371988794043)) ;
#19764 = CARTESIAN_POINT('Ctrl Pts',(-4.1,-1.66184219188422,-10.6371988794043)) ;
#19765 = CARTESIAN_POINT('Ctrl Pts',(-4.07235177185144,-1.51526219119597,
-10.6479776813726)) ;
#19766 = CARTESIAN_POINT('Ctrl Pts',(-3.9619742531141,-1.24717131941471,-10.6895386999817)) ;
#19767 = CARTESIAN_POINT('Ctrl Pts',(-3.87930809485592,-1.12560270583,-10.7201158159833)) ;
#19768 = CARTESIAN_POINT('Ctrl Pts',(-3.68673548477559,-0.929226386053517,
-10.787906168642)) ;
#19769 = CARTESIAN_POINT('Ctrl Pts',(-3.5620474526488,-0.842886484503946,
-10.8301593198666)) ;
#19770 = CARTESIAN_POINT('Ctrl Pts',(-3.28870394625325,-0.728266045313485,
-10.9162703933172)) ;
#19771 = CARTESIAN_POINT('Ctrl Pts',(-3.13999995839577,-0.7,-10.9599935484512)) ;
#19772 = CARTESIAN_POINT('Ctrl Pts',(-2.86295917531106,-0.7,-11.0355626174438)) ;
#19773 = CARTESIAN_POINT('Ctrl Pts',(-2.71564409591941,-0.727198489365921,
-11.0727078200836)) ;
#19774 = CARTESIAN_POINT('Ctrl Pts',(-2.44303520251314,-0.840025212780807,
-11.1360298274263)) ;
#19775 = CARTESIAN_POINT('Ctrl Pts',(-2.31779618826562,-0.925706392284951,
-11.1623481119451)) ;
#19776 = CARTESIAN_POINT('Ctrl Pts',(-2.18630985484209,-1.05835791598098,
-11.1884379436503)) ;
#19777 = CARTESIAN_POINT('Ctrl Pts',(-2.15513164480001,-1.09395867504312,
-11.1944756494667)) ;
#19778 = CARTESIAN_POINT('Ctrl Pts',(-2.12602916254692,-1.13203669615648,
-11.2)) ;
#19779 = CARTESIAN_POINT('',(-2.12602916254692,-0.580912236431864,-11.2)) ;
#19780 = CARTESIAN_POINT('',(-2.12602916254692,-1.8,-11.2)) ;
#19781 = CARTESIAN_POINT('',(-2.12602916254692,-3.01908776356814,-11.2)) ;
#19782 = CARTESIAN_POINT('Ctrl Pts',(-2.12602916254692,-0.580912236431864,
-11.2)) ;
#19783 = CARTESIAN_POINT('Ctrl Pts',(-2.05711563629085,-0.63031672891695,
-11.2130814434388)) ;
#19784 = CARTESIAN_POINT('Ctrl Pts',(-1.99323281619767,-0.685058529370311,
-11.2245461145188)) ;
#19785 = CARTESIAN_POINT('Ctrl Pts',(-1.86992093614613,-0.809229549581467,
-11.2457923763132)) ;
#19786 = CARTESIAN_POINT('Ctrl Pts',(-1.80806979456003,-0.88406833950675,
-11.2558400434588)) ;
#19787 = CARTESIAN_POINT('Ctrl Pts',(-1.69890438988511,-1.04715298044695,
-11.2728335098074)) ;
#19788 = CARTESIAN_POINT('Ctrl Pts',(-1.6515851116445,-1.13539399284769,-11.2797935238811)) ;
#19789 = CARTESIAN_POINT('Ctrl Pts',(-1.575538988389,-1.31954738708738,-11.2906665964395)) ;
#19790 = CARTESIAN_POINT('Ctrl Pts',(-1.54675013780201,-1.41560915257294,
-11.2945972589809)) ;
#19791 = CARTESIAN_POINT('Ctrl Pts',(-1.50897676604781,-1.6088424695419,-11.2997058524029)) ;
#19792 = CARTESIAN_POINT('Ctrl Pts',(-1.5,-1.70601550683761,-11.3008849211024)) ;
#19793 = CARTESIAN_POINT('Ctrl Pts',(-1.5,-1.8,-11.3008849211024)) ;
#19794 = CARTESIAN_POINT('Ctrl Pts',(-1.5,-1.89398449316239,-11.3008849211024)) ;
#19795 = CARTESIAN_POINT('Ctrl Pts',(-1.50897676604781,-1.9911575304581,-11.2997058524029)) ;
#19796 = CARTESIAN_POINT('Ctrl Pts',(-1.54675013780201,-2.18439084742706,
-11.2945972589809)) ;
#19797 = CARTESIAN_POINT('Ctrl Pts',(-1.575538988389,-2.28045261291263,-11.2906665964395)) ;
#19798 = CARTESIAN_POINT('Ctrl Pts',(-1.6515851116445,-2.46460600715231,-11.2797935238811)) ;
#19799 = CARTESIAN_POINT('Ctrl Pts',(-1.69890438988511,-2.55284701955305,
-11.2728335098074)) ;
#19800 = CARTESIAN_POINT('Ctrl Pts',(-1.80806979456003,-2.71593166049325,
-11.2558400434588)) ;
#19801 = CARTESIAN_POINT('Ctrl Pts',(-1.86992093614613,-2.79077045041853,
-11.2457923763132)) ;
#19802 = CARTESIAN_POINT('Ctrl Pts',(-1.99323281619761,-2.91494147062963,
-11.2245461145188)) ;
#19803 = CARTESIAN_POINT('Ctrl Pts',(-2.05711563629117,-2.96968327108328,
-11.2130814434387)) ;
#19804 = CARTESIAN_POINT('Ctrl Pts',(-2.12602916254692,-3.01908776356814,
-11.2)) ;
#19805 = CARTESIAN_POINT('',(-2.12602916254692,-1.8,-11.2)) ;
#19806 = CARTESIAN_POINT('Origin',(-2.5,-4.1,11.5)) ;
#19807 = CARTESIAN_POINT('',(-2.91,-4.6,11.5)) ;
#19808 = CARTESIAN_POINT('Origin',(-2.5,-4.6,11.5)) ;
#19809 = CARTESIAN_POINT('',(-2.91,-3.5,11.5)) ;
#19810 = CARTESIAN_POINT('',(-2.91,-4.1,11.5)) ;
#19811 = CARTESIAN_POINT('Origin',(-2.5,-3.5,11.5)) ;
#19812 = CARTESIAN_POINT('Origin',(-2.5,-3.6,11.5)) ;
#19813 = CARTESIAN_POINT('Origin',(-2.5,-3.5,11.5)) ;
#19814 = CARTESIAN_POINT('Origin',(-2.5,-3.5,11.5)) ;
#19815 = CARTESIAN_POINT('Origin',(0.,-3.6,0.)) ;
#19816 = CARTESIAN_POINT('',(7.1,-3.6,-8.)) ;
#19817 = CARTESIAN_POINT('Origin',(8.,-3.6,-8.)) ;
#19818 = CARTESIAN_POINT('Origin',(8.,-3.6,-8.)) ;
#19819 = CARTESIAN_POINT('',(-2.5,-3.6,3.06161699786838E-16)) ;
#19820 = CARTESIAN_POINT('Origin',(0.,-3.6,0.)) ;
#19821 = CARTESIAN_POINT('Origin',(5.975,-2.,-10.349003575224)) ;
#19822 = CARTESIAN_POINT('',(5.65,-4.,-10.349003575224)) ;
#19823 = CARTESIAN_POINT('Origin',(5.975,-4.,-10.349003575224)) ;
#19824 = CARTESIAN_POINT('',(5.65,-0.0999999999999999,-10.349003575224)) ;
#19825 = CARTESIAN_POINT('',(5.65,-2.,-10.349003575224)) ;
#19826 = CARTESIAN_POINT('Origin',(5.975,-0.0999999999999999,-10.349003575224)) ;
#19827 = CARTESIAN_POINT('Origin',(-5.975,-2.,-10.349003575224)) ;
#19828 = CARTESIAN_POINT('',(-6.30000000000001,-4.,-10.349003575224)) ;
#19829 = CARTESIAN_POINT('Origin',(-5.975,-4.,-10.349003575224)) ;
#19830 = CARTESIAN_POINT('',(-6.30000000000001,-0.0999999999999999,-10.349003575224)) ;
#19831 = CARTESIAN_POINT('',(-6.30000000000001,-2.,-10.349003575224)) ;
#19832 = CARTESIAN_POINT('Origin',(-5.975,-0.0999999999999999,-10.349003575224)) ;
#19833 = CARTESIAN_POINT('Origin',(-11.95,-2.,1.46345292498109E-15)) ;
#19834 = CARTESIAN_POINT('',(-12.275,-4.,1.50325394595338E-15)) ;
#19835 = CARTESIAN_POINT('Origin',(-11.95,-4.,1.46345292498109E-15)) ;
#19836 = CARTESIAN_POINT('',(-12.275,-0.0999999999999999,1.4236519040088E-15)) ;
#19837 = CARTESIAN_POINT('',(-12.275,-2.,1.50325394595338E-15)) ;
#19838 = CARTESIAN_POINT('Origin',(-11.95,-0.0999999999999999,1.46345292498109E-15)) ;
#19839 = CARTESIAN_POINT('Origin',(-5.975,-2.,10.349003575224)) ;
#19840 = CARTESIAN_POINT('',(-6.3,-4.,10.349003575224)) ;
#19841 = CARTESIAN_POINT('Origin',(-5.975,-4.,10.349003575224)) ;
#19842 = CARTESIAN_POINT('',(-6.3,-0.0999999999999999,10.349003575224)) ;
#19843 = CARTESIAN_POINT('',(-6.3,-2.,10.349003575224)) ;
#19844 = CARTESIAN_POINT('Origin',(-5.975,-0.0999999999999999,10.349003575224)) ;
#19845 = CARTESIAN_POINT('Origin',(5.975,-2.,10.349003575224)) ;
#19846 = CARTESIAN_POINT('',(5.65,-4.,10.349003575224)) ;
#19847 = CARTESIAN_POINT('Origin',(5.975,-4.,10.349003575224)) ;
#19848 = CARTESIAN_POINT('',(5.65,-0.0999999999999999,10.349003575224)) ;
#19849 = CARTESIAN_POINT('',(5.65,-2.,10.349003575224)) ;
#19850 = CARTESIAN_POINT('Origin',(5.975,-0.0999999999999999,10.349003575224)) ;
#19851 = CARTESIAN_POINT('Origin',(11.95,-2.,0.)) ;
#19852 = CARTESIAN_POINT('',(11.625,-4.,3.9801020972289E-17)) ;
#19853 = CARTESIAN_POINT('Origin',(11.95,-4.,0.)) ;
#19854 = CARTESIAN_POINT('',(11.625,-0.0999999999999999,-3.9801020972289E-17)) ;
#19855 = CARTESIAN_POINT('',(11.625,-2.,3.9801020972289E-17)) ;
#19856 = CARTESIAN_POINT('Origin',(11.95,-0.0999999999999999,0.)) ;
#19857 = CARTESIAN_POINT('Origin',(-4.,-4.1,11.25)) ;
#19858 = CARTESIAN_POINT('',(-4.,-4.,11.842719282327)) ;
#19859 = CARTESIAN_POINT('',(-4.,-3.6,11.842719282327)) ;
#19860 = CARTESIAN_POINT('',(-4.,-2.05,11.842719282327)) ;
#19861 = CARTESIAN_POINT('',(-4.,-4.,10.)) ;
#19862 = CARTESIAN_POINT('',(-4.,-4.,5.625)) ;
#19863 = CARTESIAN_POINT('',(-4.,-4.6,10.)) ;
#19864 = CARTESIAN_POINT('',(-4.,-4.1,10.)) ;
#19865 = CARTESIAN_POINT('',(-4.,-4.6,12.5)) ;
#19866 = CARTESIAN_POINT('',(-4.,-4.6,11.25)) ;
#19867 = CARTESIAN_POINT('',(-4.,-3.6,12.5)) ;
#19868 = CARTESIAN_POINT('',(-4.,-4.1,12.5)) ;
#19869 = CARTESIAN_POINT('',(-4.,-3.6,11.25)) ;
#19870 = CARTESIAN_POINT('Origin',(0.,-4.1,10.)) ;
#19871 = CARTESIAN_POINT('',(4.,-4.,10.)) ;
#19872 = CARTESIAN_POINT('',(0.,-4.,10.)) ;
#19873 = CARTESIAN_POINT('',(4.,-4.6,10.)) ;
#19874 = CARTESIAN_POINT('',(4.,-4.1,10.)) ;
#19875 = CARTESIAN_POINT('',(0.,-4.6,10.)) ;
#19876 = CARTESIAN_POINT('Origin',(0.,-3.6,11.25)) ;
#19877 = CARTESIAN_POINT('',(0.,-3.6,12.5)) ;
#19878 = CARTESIAN_POINT('Origin',(0.,-3.6,0.)) ;
#19879 = CARTESIAN_POINT('',(0.,-3.6,12.5)) ;
#19880 = CARTESIAN_POINT('Origin',(0.,-4.1,12.5)) ;
#19881 = CARTESIAN_POINT('',(4.,-4.6,12.5)) ;
#19882 = CARTESIAN_POINT('',(4.,-3.6,12.5)) ;
#19883 = CARTESIAN_POINT('',(4.,-4.1,12.5)) ;
#19884 = CARTESIAN_POINT('',(0.,-3.6,12.5)) ;
#19885 = CARTESIAN_POINT('',(0.,-4.6,12.5)) ;
#19886 = CARTESIAN_POINT('Origin',(0.,-4.6,11.25)) ;
#19887 = CARTESIAN_POINT('',(4.,-4.6,11.25)) ;
#19888 = CARTESIAN_POINT('Origin',(0.,-3.6,11.25)) ;
#19889 = CARTESIAN_POINT('',(4.,-3.6,11.842719282327)) ;
#19890 = CARTESIAN_POINT('Origin',(0.,-3.6,0.)) ;
#19891 = CARTESIAN_POINT('',(4.,-3.6,11.25)) ;
#19892 = CARTESIAN_POINT('Origin',(4.,-4.1,11.25)) ;
#19893 = CARTESIAN_POINT('',(4.,-4.,11.842719282327)) ;
#19894 = CARTESIAN_POINT('',(4.,-2.05,11.842719282327)) ;
#19895 = CARTESIAN_POINT('',(4.,-4.,5.625)) ;
#19896 = CARTESIAN_POINT('Origin',(0.,-2.05,0.)) ;
#19897 = CARTESIAN_POINT('',(-12.5,-0.0999999999999999,1.53080849893419E-15)) ;
#19898 = CARTESIAN_POINT('Origin',(0.,-0.0999999999999999,0.)) ;
#19899 = CARTESIAN_POINT('',(-12.5,-4.,1.53080849893419E-15)) ;
#19900 = CARTESIAN_POINT('',(-12.5,-2.05,1.53080849893419E-15)) ;
#19901 = CARTESIAN_POINT('Origin',(0.,-4.,0.)) ;
#19902 = CARTESIAN_POINT('',(8.97223799923196,-4.,-8.70338700076804)) ;
#19903 = CARTESIAN_POINT('Origin',(0.,-4.,0.)) ;
#19904 = CARTESIAN_POINT('',(8.97223799923192,-3.6,-8.70338700076808)) ;
#19905 = CARTESIAN_POINT('',(8.97223799923192,-4.7,-8.70338700076808)) ;
#19906 = CARTESIAN_POINT('',(8.70338700076808,-3.6,-8.97223799923192)) ;
#19907 = CARTESIAN_POINT('Origin',(0.,-3.6,0.)) ;
#19908 = CARTESIAN_POINT('',(8.70338700076804,-4.,-8.97223799923196)) ;
#19909 = CARTESIAN_POINT('',(8.70338700076808,-4.7,-8.97223799923192)) ;
#19910 = CARTESIAN_POINT('Origin',(0.,-4.,0.)) ;
#19911 = CARTESIAN_POINT('',(-1.5,-1.8,-12.4096736459909)) ;
#19912 = CARTESIAN_POINT('',(-4.5,-1.8,-11.6619037896906)) ;
#19913 = CARTESIAN_POINT('Ctrl Pts',(-1.5,-1.8,-12.4096736459909)) ;
#19914 = CARTESIAN_POINT('Ctrl Pts',(-1.5,-1.61196600654566,-12.4096736459909)) ;
#19915 = CARTESIAN_POINT('Ctrl Pts',(-1.53753764650229,-1.41147435037358,
-12.4053162844128)) ;
#19916 = CARTESIAN_POINT('Ctrl Pts',(-1.6517341137174,-1.13508183989584,-12.3904498694233)) ;
#19917 = CARTESIAN_POINT('Ctrl Pts',(-1.69911200155108,-1.04678132995196,
-12.3841054114811)) ;
#19918 = CARTESIAN_POINT('Ctrl Pts',(-1.80844505033484,-0.883569560086197,
-12.3686124903528)) ;
#19919 = CARTESIAN_POINT('Ctrl Pts',(-1.87040554697203,-0.808663104083316,
-12.3594510770994)) ;
#19920 = CARTESIAN_POINT('Ctrl Pts',(-2.00366337658874,-0.674636282719867,
-12.3385567824571)) ;
#19921 = CARTESIAN_POINT('Ctrl Pts',(-2.07973539361739,-0.611285895478787,
-12.3260595439938)) ;
#19922 = CARTESIAN_POINT('Ctrl Pts',(-2.24505223667302,-0.500006906723129,
-12.2970233651971)) ;
#19923 = CARTESIAN_POINT('Ctrl Pts',(-2.33429019684881,-0.452070861236452,
-12.2804738646022)) ;
#19924 = CARTESIAN_POINT('Ctrl Pts',(-2.51988844594125,-0.375368333774488,
-12.2437376355435)) ;
#19925 = CARTESIAN_POINT('Ctrl Pts',(-2.61639808467943,-0.346536928463552,
-12.2235131445539)) ;
#19926 = CARTESIAN_POINT('Ctrl Pts',(-2.80979164782945,-0.308850741038295,
-12.1805124452298)) ;
#19927 = CARTESIAN_POINT('Ctrl Pts',(-2.90667569879011,-0.3,-12.1577332645547)) ;
#19928 = CARTESIAN_POINT('Ctrl Pts',(-3.19117405971703,-0.3,-12.0873979601089)) ;
#19929 = CARTESIAN_POINT('Ctrl Pts',(-3.39395738819548,-0.338648265257061,
-12.0319909475619)) ;
#19930 = CARTESIAN_POINT('Ctrl Pts',(-3.76627999316394,-0.494792641049793,
-11.9206915878575)) ;
#19931 = CARTESIAN_POINT('Ctrl Pts',(-3.93590065069828,-0.61225551516906,
-11.8650249831913)) ;
#19932 = CARTESIAN_POINT('Ctrl Pts',(-4.19851097400854,-0.879581031518828,
-11.7745897312595)) ;
#19933 = CARTESIAN_POINT('Ctrl Pts',(-4.31145091679816,-1.04551443822509,
-11.7331953681633)) ;
#19934 = CARTESIAN_POINT('Ctrl Pts',(-4.42454131034426,-1.31992710340207,
-11.6908107024705)) ;
#19935 = CARTESIAN_POINT('Ctrl Pts',(-4.45323046108314,-1.41557935260616,
-11.6798607302848)) ;
#19936 = CARTESIAN_POINT('Ctrl Pts',(-4.49096465856084,-1.60847351660445,
-11.6654037501561)) ;
#19937 = CARTESIAN_POINT('Ctrl Pts',(-4.5,-1.70571785795988,-11.6619037896906)) ;
#19938 = CARTESIAN_POINT('Ctrl Pts',(-4.5,-1.8,-11.6619037896906)) ;
#19939 = CARTESIAN_POINT('Ctrl Pts',(-4.5,-1.8,-11.6619037896906)) ;
#19940 = CARTESIAN_POINT('Ctrl Pts',(-4.5,-1.89428214204012,-11.6619037896906)) ;
#19941 = CARTESIAN_POINT('Ctrl Pts',(-4.49096465856084,-1.99152648339555,
-11.6654037501561)) ;
#19942 = CARTESIAN_POINT('Ctrl Pts',(-4.45323046108314,-2.18442064739384,
-11.6798607302848)) ;
#19943 = CARTESIAN_POINT('Ctrl Pts',(-4.42454131034426,-2.28007289659793,
-11.6908107024705)) ;
#19944 = CARTESIAN_POINT('Ctrl Pts',(-4.31145091679816,-2.55448556177491,
-11.7331953681633)) ;
#19945 = CARTESIAN_POINT('Ctrl Pts',(-4.19851097400854,-2.72041896848117,
-11.7745897312595)) ;
#19946 = CARTESIAN_POINT('Ctrl Pts',(-3.93590065069828,-2.98774448483094,
-11.8650249831913)) ;
#19947 = CARTESIAN_POINT('Ctrl Pts',(-3.76627999316394,-3.10520735895021,
-11.9206915878575)) ;
#19948 = CARTESIAN_POINT('Ctrl Pts',(-3.39395738819548,-3.26135173474294,
-12.0319909475619)) ;
#19949 = CARTESIAN_POINT('Ctrl Pts',(-3.19117405971703,-3.3,-12.0873979601089)) ;
#19950 = CARTESIAN_POINT('Ctrl Pts',(-2.90667569879011,-3.3,-12.1577332645547)) ;
#19951 = CARTESIAN_POINT('Ctrl Pts',(-2.80979164782945,-3.29114925896171,
-12.1805124452298)) ;
#19952 = CARTESIAN_POINT('Ctrl Pts',(-2.61639808467943,-3.25346307153645,
-12.2235131445539)) ;
#19953 = CARTESIAN_POINT('Ctrl Pts',(-2.51988844594125,-3.22463166622551,
-12.2437376355435)) ;
#19954 = CARTESIAN_POINT('Ctrl Pts',(-2.33429019684881,-3.14792913876355,
-12.2804738646022)) ;
#19955 = CARTESIAN_POINT('Ctrl Pts',(-2.24505223667302,-3.09999309327687,
-12.2970233651971)) ;
#19956 = CARTESIAN_POINT('Ctrl Pts',(-2.07973539361739,-2.98871410452121,
-12.3260595439938)) ;
#19957 = CARTESIAN_POINT('Ctrl Pts',(-2.00366337658874,-2.92536371728013,
-12.3385567824571)) ;
#19958 = CARTESIAN_POINT('Ctrl Pts',(-1.87040554697204,-2.79133689591668,
-12.3594510770994)) ;
#19959 = CARTESIAN_POINT('Ctrl Pts',(-1.80844505033484,-2.7164304399138,-12.3686124903528)) ;
#19960 = CARTESIAN_POINT('Ctrl Pts',(-1.69911200155108,-2.55321867004804,
-12.3841054114811)) ;
#19961 = CARTESIAN_POINT('Ctrl Pts',(-1.6517341137174,-2.46491816010416,-12.3904498694233)) ;
#19962 = CARTESIAN_POINT('Ctrl Pts',(-1.53753764650229,-2.18852564962642,
-12.4053162844128)) ;
#19963 = CARTESIAN_POINT('Ctrl Pts',(-1.5,-1.98803399345434,-12.4096736459909)) ;
#19964 = CARTESIAN_POINT('Ctrl Pts',(-1.5,-1.8,-12.4096736459909)) ;
#19965 = CARTESIAN_POINT('Origin',(-3.,-1.8,-11.5)) ;
#19966 = CARTESIAN_POINT('',(-4.1,-1.8,-13.)) ;
#19967 = CARTESIAN_POINT('Origin',(-3.,-1.8,-13.)) ;
#19968 = CARTESIAN_POINT('',(-4.1,-1.8,-11.5)) ;
#19969 = CARTESIAN_POINT('Origin',(-3.,-1.8,-11.2)) ;
#19970 = CARTESIAN_POINT('Origin',(-3.,-1.8,-12.1)) ;
#19971 = CARTESIAN_POINT('',(-4.5,-1.8,-13.)) ;
#19972 = CARTESIAN_POINT('',(-4.5,-1.8,-12.1)) ;
#19973 = CARTESIAN_POINT('Origin',(-3.,-1.8,-13.)) ;
#19974 = CARTESIAN_POINT('Origin',(-3.,-1.8,-12.1)) ;
#19975 = CARTESIAN_POINT('Origin',(-3.,-1.8,-11.2)) ;
#19976 = CARTESIAN_POINT('Origin',(-3.,-1.8,-13.)) ;
#19977 = CARTESIAN_POINT('Origin',(-3.,-1.8,-11.2)) ;
#19978 = CARTESIAN_POINT('Origin',(8.,-3.,-8.)) ;
#19979 = CARTESIAN_POINT('Origin',(8.,-3.,-8.)) ;
#19980 = CARTESIAN_POINT('Origin',(8.,-4.65,-8.)) ;
#19981 = CARTESIAN_POINT('',(7.1,-5.8,-8.)) ;
#19982 = CARTESIAN_POINT('Origin',(8.,-5.8,-8.)) ;
#19983 = CARTESIAN_POINT('',(7.1,-4.65,-8.)) ;
#19984 = CARTESIAN_POINT('Origin',(8.,-3.6,-8.)) ;
#19985 = CARTESIAN_POINT('Origin',(8.,-3.6,-8.)) ;
#19986 = CARTESIAN_POINT('Origin',(8.,-4.7,-8.)) ;
#19987 = CARTESIAN_POINT('',(6.8,-4.,-8.)) ;
#19988 = CARTESIAN_POINT('Origin',(8.,-4.,-8.)) ;
#19989 = CARTESIAN_POINT('',(6.8,-5.8,-8.)) ;
#19990 = CARTESIAN_POINT('',(6.8,-4.7,-8.)) ;
#19991 = CARTESIAN_POINT('Origin',(8.,-5.8,-8.)) ;
#19992 = CARTESIAN_POINT('Origin',(8.,-4.,-8.)) ;
#19993 = CARTESIAN_POINT('Origin',(8.,-5.8,-8.)) ;
#19994 = CARTESIAN_POINT('Origin',(0.,-4.,0.)) ;
#19995 = CARTESIAN_POINT('',(-2.5,-4.,3.06161699786838E-16)) ;
#19996 = CARTESIAN_POINT('Origin',(0.,-4.,0.)) ;
#19997 = CARTESIAN_POINT('Origin',(0.,-3.8,0.)) ;
#19998 = CARTESIAN_POINT('',(-1.5,-4.,1.83697019872103E-16)) ;
#19999 = CARTESIAN_POINT('Origin',(0.,-4.,0.)) ;
#20000 = CARTESIAN_POINT('',(-1.5,-3.6,-1.83697019872103E-16)) ;
#20001 = CARTESIAN_POINT('',(-1.5,-3.8,1.83697019872103E-16)) ;
#20002 = CARTESIAN_POINT('Origin',(0.,-3.6,0.)) ;
#20003 = CARTESIAN_POINT('Origin',(0.,-2.95,0.)) ;
#20004 = CARTESIAN_POINT('',(-1.75,-3.6,2.14313189850787E-16)) ;
#20005 = CARTESIAN_POINT('Origin',(0.,-3.6,0.)) ;
#20006 = CARTESIAN_POINT('',(-1.75,-2.4,-2.14313189850787E-16)) ;
#20007 = CARTESIAN_POINT('',(-1.75,-2.95,2.14313189850787E-16)) ;
#20008 = CARTESIAN_POINT('Origin',(0.,-2.4,0.)) ;
#20009 = CARTESIAN_POINT('Origin',(0.,-3.6,0.)) ;
#20010 = CARTESIAN_POINT('Origin',(0.,-4.85,0.)) ;
#20011 = CARTESIAN_POINT('',(-1.75,-5.6,2.14313189850787E-16)) ;
#20012 = CARTESIAN_POINT('Origin',(0.,-5.6,0.)) ;
#20013 = CARTESIAN_POINT('',(-1.75,-4.,2.14313189850787E-16)) ;
#20014 = CARTESIAN_POINT('',(-1.75,-4.85,2.14313189850787E-16)) ;
#20015 = CARTESIAN_POINT('Origin',(0.,-4.,0.)) ;
#20016 = CARTESIAN_POINT('Origin',(0.,-4.,0.)) ;
#20017 = CARTESIAN_POINT('Origin',(0.,-3.,0.)) ;
#20018 = CARTESIAN_POINT('',(-2.5,-2.4,3.06161699786838E-16)) ;
#20019 = CARTESIAN_POINT('Origin',(0.,-2.4,0.)) ;
#20020 = CARTESIAN_POINT('',(-2.5,-3.,3.06161699786838E-16)) ;
#20021 = CARTESIAN_POINT('Origin',(0.,-2.4,0.)) ;
#20022 = CARTESIAN_POINT('Origin',(0.,-4.6,0.)) ;
#20023 = CARTESIAN_POINT('',(-2.5,-5.6,3.06161699786838E-16)) ;
#20024 = CARTESIAN_POINT('',(-2.5,-4.6,3.06161699786838E-16)) ;
#20025 = CARTESIAN_POINT('Origin',(0.,-5.6,0.)) ;
#20026 = CARTESIAN_POINT('Origin',(0.,-5.6,0.)) ;
#20027 = CARTESIAN_POINT('Origin',(0.,-0.0999999999999999,0.)) ;
#20028 = CARTESIAN_POINT('',(0.,0.,0.)) ;
#20029 = CARTESIAN_POINT('Origin',(-6.1946255125913,3.75,8.84684207832111)) ;
#20030 = CARTESIAN_POINT('',(-6.3971255125913,3.6,8.84684207832111)) ;
#20031 = CARTESIAN_POINT('Origin',(-6.1946255125913,3.6,8.84684207832111)) ;
#20032 = CARTESIAN_POINT('',(-6.3971255125913,4.,8.84684207832111)) ;
#20033 = CARTESIAN_POINT('',(-6.3971255125913,3.75,8.84684207832111)) ;
#20034 = CARTESIAN_POINT('Origin',(-6.1946255125913,4.,8.84684207832111)) ;
#20035 = CARTESIAN_POINT('Origin',(5.975,2.,-10.349003575224)) ;
#20036 = CARTESIAN_POINT('',(5.65,0.0999999999999999,-10.349003575224)) ;
#20037 = CARTESIAN_POINT('Origin',(5.975,0.0999999999999999,-10.349003575224)) ;
#20038 = CARTESIAN_POINT('',(5.65,4.,-10.349003575224)) ;
#20039 = CARTESIAN_POINT('',(5.65,2.,-10.349003575224)) ;
#20040 = CARTESIAN_POINT('Origin',(5.975,4.,-10.349003575224)) ;
#20041 = CARTESIAN_POINT('Origin',(-5.975,2.,-10.349003575224)) ;
#20042 = CARTESIAN_POINT('',(-6.30000000000001,0.0999999999999999,-10.349003575224)) ;
#20043 = CARTESIAN_POINT('Origin',(-5.975,0.0999999999999999,-10.349003575224)) ;
#20044 = CARTESIAN_POINT('',(-6.30000000000001,4.,-10.349003575224)) ;
#20045 = CARTESIAN_POINT('',(-6.30000000000001,2.,-10.349003575224)) ;
#20046 = CARTESIAN_POINT('Origin',(-5.975,4.,-10.349003575224)) ;
#20047 = CARTESIAN_POINT('Origin',(-11.95,2.,1.46345292498109E-15)) ;
#20048 = CARTESIAN_POINT('',(-12.275,0.0999999999999999,1.50325394595338E-15)) ;
#20049 = CARTESIAN_POINT('Origin',(-11.95,0.0999999999999999,1.46345292498109E-15)) ;
#20050 = CARTESIAN_POINT('',(-12.275,4.,1.4236519040088E-15)) ;
#20051 = CARTESIAN_POINT('',(-12.275,2.,1.50325394595338E-15)) ;
#20052 = CARTESIAN_POINT('Origin',(-11.95,4.,1.46345292498109E-15)) ;
#20053 = CARTESIAN_POINT('Origin',(-5.975,2.,10.349003575224)) ;
#20054 = CARTESIAN_POINT('',(-6.3,0.0999999999999999,10.349003575224)) ;
#20055 = CARTESIAN_POINT('Origin',(-5.975,0.0999999999999999,10.349003575224)) ;
#20056 = CARTESIAN_POINT('',(-6.3,4.,10.349003575224)) ;
#20057 = CARTESIAN_POINT('',(-6.3,2.,10.349003575224)) ;
#20058 = CARTESIAN_POINT('Origin',(-5.975,4.,10.349003575224)) ;
#20059 = CARTESIAN_POINT('Origin',(5.975,2.,10.349003575224)) ;
#20060 = CARTESIAN_POINT('',(5.65,0.0999999999999999,10.349003575224)) ;
#20061 = CARTESIAN_POINT('Origin',(5.975,0.0999999999999999,10.349003575224)) ;
#20062 = CARTESIAN_POINT('',(5.65,4.,10.349003575224)) ;
#20063 = CARTESIAN_POINT('',(5.65,2.,10.349003575224)) ;
#20064 = CARTESIAN_POINT('Origin',(5.975,4.,10.349003575224)) ;
#20065 = CARTESIAN_POINT('Origin',(11.95,2.,0.)) ;
#20066 = CARTESIAN_POINT('',(11.625,0.0999999999999999,3.9801020972289E-17)) ;
#20067 = CARTESIAN_POINT('Origin',(11.95,0.0999999999999999,0.)) ;
#20068 = CARTESIAN_POINT('',(11.625,4.,-3.9801020972289E-17)) ;
#20069 = CARTESIAN_POINT('',(11.625,2.,3.9801020972289E-17)) ;
#20070 = CARTESIAN_POINT('Origin',(11.95,4.,0.)) ;
#20071 = CARTESIAN_POINT('Origin',(1.59756323453576,3.65,-9.06023132771231)) ;
#20072 = CARTESIAN_POINT('',(0.187563234535756,3.6,-9.06023132771231)) ;
#20073 = CARTESIAN_POINT('Origin',(1.59756323453576,3.6,-9.06023132771231)) ;
#20074 = CARTESIAN_POINT('',(0.187563234535756,4.2,-9.06023132771231)) ;
#20075 = CARTESIAN_POINT('',(0.187563234535756,3.65,-9.06023132771231)) ;
#20076 = CARTESIAN_POINT('Origin',(1.59756323453576,4.2,-9.06023132771231)) ;
#20077 = CARTESIAN_POINT('Origin',(1.59756323453576,3.9,-9.06023132771231)) ;
#20078 = CARTESIAN_POINT('',(-0.202436765464244,4.2,-9.06023132771231)) ;
#20079 = CARTESIAN_POINT('Origin',(1.59756323453576,4.2,-9.06023132771231)) ;
#20080 = CARTESIAN_POINT('',(-0.202436765464244,4.,-9.06023132771231)) ;
#20081 = CARTESIAN_POINT('',(-0.202436765464244,3.9,-9.06023132771231)) ;
#20082 = CARTESIAN_POINT('Origin',(1.59756323453576,4.,-9.06023132771231)) ;
#20083 = CARTESIAN_POINT('Origin',(1.59756323453576,4.2,-9.06023132771231)) ;
#20084 = CARTESIAN_POINT('Origin',(-8.33803164073718,3.65,3.88808800801444)) ;
#20085 = CARTESIAN_POINT('',(-9.74803164073718,3.6,3.88808800801444)) ;
#20086 = CARTESIAN_POINT('Origin',(-8.33803164073718,3.6,3.88808800801444)) ;
#20087 = CARTESIAN_POINT('',(-9.74803164073718,4.2,3.88808800801444)) ;
#20088 = CARTESIAN_POINT('',(-9.74803164073718,3.65,3.88808800801444)) ;
#20089 = CARTESIAN_POINT('Origin',(-8.33803164073718,4.2,3.88808800801444)) ;
#20090 = CARTESIAN_POINT('Origin',(-8.33803164073718,3.9,3.88808800801444)) ;
#20091 = CARTESIAN_POINT('',(-10.1380316407372,4.2,3.88808800801444)) ;
#20092 = CARTESIAN_POINT('Origin',(-8.33803164073718,4.2,3.88808800801444)) ;
#20093 = CARTESIAN_POINT('',(-10.1380316407372,4.,3.88808800801444)) ;
#20094 = CARTESIAN_POINT('',(-10.1380316407372,3.9,3.88808800801444)) ;
#20095 = CARTESIAN_POINT('Origin',(-8.33803164073718,4.,3.88808800801444)) ;
#20096 = CARTESIAN_POINT('Origin',(-8.33803164073718,4.2,3.88808800801444)) ;
#20097 = CARTESIAN_POINT('Origin',(0.,3.9,0.)) ;
#20098 = CARTESIAN_POINT('',(-5.9,3.7,7.22541611496938E-16)) ;
#20099 = CARTESIAN_POINT('Origin',(0.,3.7,0.)) ;
#20100 = CARTESIAN_POINT('',(-5.9,4.,-7.22541611496938E-16)) ;
#20101 = CARTESIAN_POINT('',(-5.9,3.9,7.22541611496938E-16)) ;
#20102 = CARTESIAN_POINT('Origin',(0.,4.,0.)) ;
#20103 = CARTESIAN_POINT('Origin',(0.,3.7,0.)) ;
#20104 = CARTESIAN_POINT('',(-5.5,3.7,6.73555739531044E-16)) ;
#20105 = CARTESIAN_POINT('Origin',(0.,3.7,0.)) ;
#20106 = CARTESIAN_POINT('Origin',(0.,3.8,0.)) ;
#20107 = CARTESIAN_POINT('',(-5.5,3.6,6.73555739531044E-16)) ;
#20108 = CARTESIAN_POINT('Origin',(0.,3.6,0.)) ;
#20109 = CARTESIAN_POINT('',(-5.5,3.8,6.73555739531044E-16)) ;
#20110 = CARTESIAN_POINT('Origin',(0.,1.8,0.)) ;
#20111 = CARTESIAN_POINT('',(-11.4,0.0999999999999999,1.39609735102798E-15)) ;
#20112 = CARTESIAN_POINT('Origin',(0.,0.0999999999999999,0.)) ;
#20113 = CARTESIAN_POINT('',(-11.4,3.6,1.39609735102798E-15)) ;
#20114 = CARTESIAN_POINT('',(-11.4,1.8,1.39609735102798E-15)) ;
#20115 = CARTESIAN_POINT('Origin',(0.,3.6,0.)) ;
#20116 = CARTESIAN_POINT('Origin',(0.,3.6,0.)) ;
#20117 = CARTESIAN_POINT('Origin',(0.,2.05,0.)) ;
#20118 = CARTESIAN_POINT('',(-12.5,4.,1.53080849893419E-15)) ;
#20119 = CARTESIAN_POINT('Origin',(0.,4.,0.)) ;
#20120 = CARTESIAN_POINT('',(-12.5,0.0999999999999999,1.53080849893419E-15)) ;
#20121 = CARTESIAN_POINT('',(-12.5,2.05,1.53080849893419E-15)) ;
#20122 = CARTESIAN_POINT('Origin',(0.,0.0999999999999999,0.)) ;
#20123 = CARTESIAN_POINT('Origin',(0.,0.0999999999999999,0.)) ;
#20124 = CARTESIAN_POINT('Origin',(0.,4.,0.)) ;
#20125 = CARTESIAN_POINT('',(0.,0.,0.)) ;
#20126 = CARTESIAN_POINT('Origin',(0.,3.85,0.)) ;
#20127 = CARTESIAN_POINT('',(-5.89,4.,7.21316964697791E-16)) ;
#20128 = CARTESIAN_POINT('Origin',(0.,4.,0.)) ;
#20129 = CARTESIAN_POINT('',(-5.89,3.7,7.21316964697791E-16)) ;
#20130 = CARTESIAN_POINT('',(-5.89,3.85,7.21316964697791E-16)) ;
#20131 = CARTESIAN_POINT('Origin',(0.,3.7,0.)) ;
#20132 = CARTESIAN_POINT('Origin',(0.,3.7,0.)) ;
#20133 = CARTESIAN_POINT('Origin',(0.,4.,0.)) ;
#20134 = CARTESIAN_POINT('',(0.,0.,0.)) ;
#20135 = CARTESIAN_POINT('Origin',(5.975,0.,-10.349003575224)) ;
#20136 = CARTESIAN_POINT('',(5.65,-0.1,-10.349003575224)) ;
#20137 = CARTESIAN_POINT('Origin',(5.975,-0.1,-10.349003575224)) ;
#20138 = CARTESIAN_POINT('',(5.65,0.1,-10.349003575224)) ;
#20139 = CARTESIAN_POINT('',(5.65,0.,-10.349003575224)) ;
#20140 = CARTESIAN_POINT('Origin',(5.975,0.1,-10.349003575224)) ;
#20141 = CARTESIAN_POINT('Origin',(-5.975,0.,-10.349003575224)) ;
#20142 = CARTESIAN_POINT('',(-6.30000000000001,-0.1,-10.349003575224)) ;
#20143 = CARTESIAN_POINT('Origin',(-5.975,-0.1,-10.349003575224)) ;
#20144 = CARTESIAN_POINT('',(-6.30000000000001,0.1,-10.349003575224)) ;
#20145 = CARTESIAN_POINT('',(-6.30000000000001,0.,-10.349003575224)) ;
#20146 = CARTESIAN_POINT('Origin',(-5.975,0.1,-10.349003575224)) ;
#20147 = CARTESIAN_POINT('Origin',(-11.95,0.,1.46345292498109E-15)) ;
#20148 = CARTESIAN_POINT('',(-12.275,-0.1,1.50325394595338E-15)) ;
#20149 = CARTESIAN_POINT('Origin',(-11.95,-0.1,1.46345292498109E-15)) ;
#20150 = CARTESIAN_POINT('',(-12.275,0.1,1.4236519040088E-15)) ;
#20151 = CARTESIAN_POINT('',(-12.275,0.,1.50325394595338E-15)) ;
#20152 = CARTESIAN_POINT('Origin',(-11.95,0.1,1.46345292498109E-15)) ;
#20153 = CARTESIAN_POINT('Origin',(-5.975,0.,10.349003575224)) ;
#20154 = CARTESIAN_POINT('',(-6.3,-0.1,10.349003575224)) ;
#20155 = CARTESIAN_POINT('Origin',(-5.975,-0.1,10.349003575224)) ;
#20156 = CARTESIAN_POINT('',(-6.3,0.1,10.349003575224)) ;
#20157 = CARTESIAN_POINT('',(-6.3,0.,10.349003575224)) ;
#20158 = CARTESIAN_POINT('Origin',(-5.975,0.1,10.349003575224)) ;
#20159 = CARTESIAN_POINT('Origin',(5.975,0.,10.349003575224)) ;
#20160 = CARTESIAN_POINT('',(5.65,-0.1,10.349003575224)) ;
#20161 = CARTESIAN_POINT('Origin',(5.975,-0.1,10.349003575224)) ;
#20162 = CARTESIAN_POINT('',(5.65,0.1,10.349003575224)) ;
#20163 = CARTESIAN_POINT('',(5.65,0.,10.349003575224)) ;
#20164 = CARTESIAN_POINT('Origin',(5.975,0.1,10.349003575224)) ;
#20165 = CARTESIAN_POINT('Origin',(11.95,0.,0.)) ;
#20166 = CARTESIAN_POINT('',(11.625,-0.1,3.9801020972289E-17)) ;
#20167 = CARTESIAN_POINT('Origin',(11.95,-0.1,0.)) ;
#20168 = CARTESIAN_POINT('',(11.625,0.1,-3.9801020972289E-17)) ;
#20169 = CARTESIAN_POINT('',(11.625,0.,3.9801020972289E-17)) ;
#20170 = CARTESIAN_POINT('Origin',(11.95,0.1,0.)) ;
#20171 = CARTESIAN_POINT('Origin',(0.,0.,0.)) ;
#20172 = CARTESIAN_POINT('',(-11.4,-0.1,1.39609735102798E-15)) ;
#20173 = CARTESIAN_POINT('Origin',(0.,-0.1,0.)) ;
#20174 = CARTESIAN_POINT('',(-11.4,0.1,-1.39609735102798E-15)) ;
#20175 = CARTESIAN_POINT('',(-11.4,0.,1.39609735102798E-15)) ;
#20176 = CARTESIAN_POINT('Origin',(0.,0.1,0.)) ;
#20177 = CARTESIAN_POINT('Origin',(0.,0.,0.)) ;
#20178 = CARTESIAN_POINT('',(-12.5,0.1,1.53080849893419E-15)) ;
#20179 = CARTESIAN_POINT('Origin',(0.,0.1,0.)) ;
#20180 = CARTESIAN_POINT('',(-12.5,-0.1,1.53080849893419E-15)) ;
#20181 = CARTESIAN_POINT('',(-12.5,0.,1.53080849893419E-15)) ;
#20182 = CARTESIAN_POINT('Origin',(0.,-0.1,0.)) ;
#20183 = CARTESIAN_POINT('Origin',(0.,-0.1,0.)) ;
#20184 = CARTESIAN_POINT('Origin',(0.,0.1,0.)) ;
#20185 = CARTESIAN_POINT('',(0.,0.,0.)) ;
#20186 = CARTESIAN_POINT('Origin',(0.65,-6.2,0.252)) ;
#20187 = CARTESIAN_POINT('',(0.5,-6.8,0.252)) ;
#20188 = CARTESIAN_POINT('',(0.706396489232499,-6.8,0.252)) ;
#20189 = CARTESIAN_POINT('',(0.325,-6.8,0.252)) ;
#20190 = CARTESIAN_POINT('',(0.5,-5.5,0.252)) ;
#20191 = CARTESIAN_POINT('',(0.5,-6.2,0.252)) ;
#20192 = CARTESIAN_POINT('',(0.706396489232499,-5.5,0.252)) ;
#20193 = CARTESIAN_POINT('',(0.65,-5.5,0.252)) ;
#20194 = CARTESIAN_POINT('',(0.706396489232499,-3.9,0.252)) ;
#20195 = CARTESIAN_POINT('Origin',(0.65,-5.5,0.)) ;
#20196 = CARTESIAN_POINT('',(0.706396489232499,-5.5,-0.252)) ;
#20197 = CARTESIAN_POINT('Origin',(0.,-5.5,0.)) ;
#20198 = CARTESIAN_POINT('',(0.5,-5.5,-0.252)) ;
#20199 = CARTESIAN_POINT('',(0.5,-5.5,0.)) ;
#20200 = CARTESIAN_POINT('',(0.65,-5.5,-0.252)) ;
#20201 = CARTESIAN_POINT('Origin',(0.65,-6.2,-0.252)) ;
#20202 = CARTESIAN_POINT('',(0.706396489232499,-6.8,-0.252)) ;
#20203 = CARTESIAN_POINT('',(0.5,-6.8,-0.252)) ;
#20204 = CARTESIAN_POINT('',(0.325,-6.8,-0.252)) ;
#20205 = CARTESIAN_POINT('',(0.706396489232499,-3.9,-0.252)) ;
#20206 = CARTESIAN_POINT('',(0.5,-6.2,-0.252)) ;
#20207 = CARTESIAN_POINT('Origin',(0.5,-6.2,0.)) ;
#20208 = CARTESIAN_POINT('',(0.5,-6.8,0.)) ;
#20209 = CARTESIAN_POINT('Origin',(0.,-3.9,0.)) ;
#20210 = CARTESIAN_POINT('',(-0.75,-5.3,-9.18485099360515E-17)) ;
#20211 = CARTESIAN_POINT('Origin',(0.,-5.3,0.)) ;
#20212 = CARTESIAN_POINT('',(-0.75,-6.8,9.18485099360515E-17)) ;
#20213 = CARTESIAN_POINT('',(-0.75,-3.9,9.18485099360515E-17)) ;
#20214 = CARTESIAN_POINT('Origin',(0.,-6.8,0.)) ;
#20215 = CARTESIAN_POINT('Origin',(0.,-6.8,0.)) ;
#20216 = CARTESIAN_POINT('Origin',(0.,-5.25,0.)) ;
#20217 = CARTESIAN_POINT('',(-0.7,-5.2,-8.57252759403147E-17)) ;
#20218 = CARTESIAN_POINT('Origin',(0.,-5.2,0.)) ;
#20219 = CARTESIAN_POINT('',(-0.7,-5.3,8.57252759403147E-17)) ;
#20220 = CARTESIAN_POINT('',(-0.7,-5.25,8.57252759403147E-17)) ;
#20221 = CARTESIAN_POINT('Origin',(0.,-5.3,0.)) ;
#20222 = CARTESIAN_POINT('Origin',(0.,-5.3,0.)) ;
#20223 = CARTESIAN_POINT('Origin',(0.,-5.2,0.)) ;
#20224 = CARTESIAN_POINT('',(-0.75,-5.2,9.18485099360515E-17)) ;
#20225 = CARTESIAN_POINT('Origin',(0.,-5.2,0.)) ;
#20226 = CARTESIAN_POINT('Origin',(0.,-3.9,0.)) ;
#20227 = CARTESIAN_POINT('',(-0.75,-1.4,-9.18485099360515E-17)) ;
#20228 = CARTESIAN_POINT('Origin',(0.,-1.4,0.)) ;
#20229 = CARTESIAN_POINT('',(-0.75,-3.9,9.18485099360515E-17)) ;
#20230 = CARTESIAN_POINT('Origin',(1.55884572681199,-1.2,-0.900000000000001)) ;
#20231 = CARTESIAN_POINT('',(1.36384572681199,-1.4,-0.900000000000001)) ;
#20232 = CARTESIAN_POINT('Origin',(1.55884572681199,-1.4,-0.900000000000001)) ;
#20233 = CARTESIAN_POINT('',(1.36384572681199,-1.,-0.900000000000001)) ;
#20234 = CARTESIAN_POINT('',(1.36384572681199,-1.2,-0.900000000000001)) ;
#20235 = CARTESIAN_POINT('Origin',(1.55884572681199,-1.,-0.900000000000001)) ;
#20236 = CARTESIAN_POINT('Origin',(-1.55884572681199,-1.2,-0.9)) ;
#20237 = CARTESIAN_POINT('',(-1.75384572681199,-1.4,-0.9)) ;
#20238 = CARTESIAN_POINT('Origin',(-1.55884572681199,-1.4,-0.9)) ;
#20239 = CARTESIAN_POINT('',(-1.75384572681199,-1.,-0.9)) ;
#20240 = CARTESIAN_POINT('',(-1.75384572681199,-1.2,-0.9)) ;
#20241 = CARTESIAN_POINT('Origin',(-1.55884572681199,-1.,-0.9)) ;
#20242 = CARTESIAN_POINT('Origin',(1.10218211923262E-16,-1.2,1.8)) ;
#20243 = CARTESIAN_POINT('',(-0.195,-1.4,1.8)) ;
#20244 = CARTESIAN_POINT('Origin',(1.10218211923262E-16,-1.4,1.8)) ;
#20245 = CARTESIAN_POINT('',(-0.195,-1.,1.8)) ;
#20246 = CARTESIAN_POINT('',(-0.195,-1.2,1.8)) ;
#20247 = CARTESIAN_POINT('Origin',(1.10218211923262E-16,-1.,1.8)) ;
#20248 = CARTESIAN_POINT('Origin',(0.,-1.4,0.)) ;
#20249 = CARTESIAN_POINT('',(-2.5,-1.4,3.06161699786838E-16)) ;
#20250 = CARTESIAN_POINT('Origin',(0.,-1.4,0.)) ;
#20251 = CARTESIAN_POINT('Origin',(0.,-1.2,0.)) ;
#20252 = CARTESIAN_POINT('',(-2.5,-1.,3.06161699786838E-16)) ;
#20253 = CARTESIAN_POINT('Origin',(0.,-1.,0.)) ;
#20254 = CARTESIAN_POINT('',(-2.5,-1.2,3.06161699786838E-16)) ;
#20255 = CARTESIAN_POINT('Origin',(0.,-0.1,0.)) ;
#20256 = CARTESIAN_POINT('',(-0.5,0.8,6.12323399573677E-17)) ;
#20257 = CARTESIAN_POINT('Origin',(0.,0.8,0.)) ;
#20258 = CARTESIAN_POINT('',(-0.5,-1.,6.12323399573677E-17)) ;
#20259 = CARTESIAN_POINT('',(-0.5,-0.1,6.12323399573677E-17)) ;
#20260 = CARTESIAN_POINT('Origin',(0.,-1.,0.)) ;
#20261 = CARTESIAN_POINT('Origin',(0.,0.8,0.)) ;
#20262 = CARTESIAN_POINT('Origin',(0.,-6.8,0.)) ;
#20263 = CARTESIAN_POINT('Origin',(0.,-1.,0.)) ;
#20264 = CARTESIAN_POINT('',(0.,0.,0.)) ;
#20265 = CARTESIAN_POINT('Origin',(8.72471478008953,-0.95,-1.14863049153645)) ;
#20266 = CARTESIAN_POINT('',(8.57471478008953,-1.,-1.14863049153645)) ;
#20267 = CARTESIAN_POINT('Origin',(8.72471478008953,-1.,-1.14863049153645)) ;
#20268 = CARTESIAN_POINT('',(8.57471478008953,-0.8,-1.14863049153645)) ;
#20269 = CARTESIAN_POINT('',(8.57471478008953,-0.95,-1.14863049153645)) ;
#20270 = CARTESIAN_POINT('Origin',(8.72471478008953,-0.8,-1.14863049153645)) ;
#20271 = CARTESIAN_POINT('Origin',(8.72471478008953,-0.8,-1.14863049153645)) ;
#20272 = CARTESIAN_POINT('Origin',(8.13013988609933,-0.95,-3.36761420481279)) ;
#20273 = CARTESIAN_POINT('',(7.98013988609932,-1.,-3.36761420481279)) ;
#20274 = CARTESIAN_POINT('Origin',(8.13013988609933,-1.,-3.36761420481279)) ;
#20275 = CARTESIAN_POINT('',(7.98013988609932,-0.8,-3.36761420481279)) ;
#20276 = CARTESIAN_POINT('',(7.98013988609932,-0.95,-3.36761420481279)) ;
#20277 = CARTESIAN_POINT('Origin',(8.13013988609933,-0.8,-3.36761420481279)) ;
#20278 = CARTESIAN_POINT('Origin',(8.13013988609933,-0.8,-3.36761420481279)) ;
#20279 = CARTESIAN_POINT('Origin',(6.98150939456287,-0.95,-5.35710057527674)) ;
#20280 = CARTESIAN_POINT('',(6.83150939456287,-1.,-5.35710057527674)) ;
#20281 = CARTESIAN_POINT('Origin',(6.98150939456287,-1.,-5.35710057527674)) ;
#20282 = CARTESIAN_POINT('',(6.83150939456287,-0.8,-5.35710057527674)) ;
#20283 = CARTESIAN_POINT('',(6.83150939456287,-0.95,-5.35710057527674)) ;
#20284 = CARTESIAN_POINT('Origin',(6.98150939456287,-0.8,-5.35710057527674)) ;
#20285 = CARTESIAN_POINT('Origin',(6.98150939456287,-0.8,-5.35710057527674)) ;
#20286 = CARTESIAN_POINT('Origin',(5.35710057527674,-0.95,-6.98150939456287)) ;
#20287 = CARTESIAN_POINT('',(5.20710057527674,-1.,-6.98150939456287)) ;
#20288 = CARTESIAN_POINT('Origin',(5.35710057527674,-1.,-6.98150939456287)) ;
#20289 = CARTESIAN_POINT('',(5.20710057527674,-0.8,-6.98150939456287)) ;
#20290 = CARTESIAN_POINT('',(5.20710057527674,-0.95,-6.98150939456287)) ;
#20291 = CARTESIAN_POINT('Origin',(5.35710057527674,-0.8,-6.98150939456287)) ;
#20292 = CARTESIAN_POINT('Origin',(5.35710057527674,-0.8,-6.98150939456287)) ;
#20293 = CARTESIAN_POINT('Origin',(3.36761420481279,-0.95,-8.13013988609932)) ;
#20294 = CARTESIAN_POINT('',(3.21761420481279,-1.,-8.13013988609932)) ;
#20295 = CARTESIAN_POINT('Origin',(3.36761420481279,-1.,-8.13013988609932)) ;
#20296 = CARTESIAN_POINT('',(3.21761420481279,-0.8,-8.13013988609932)) ;
#20297 = CARTESIAN_POINT('',(3.21761420481279,-0.95,-8.13013988609932)) ;
#20298 = CARTESIAN_POINT('Origin',(3.36761420481279,-0.8,-8.13013988609932)) ;
#20299 = CARTESIAN_POINT('Origin',(3.36761420481279,-0.8,-8.13013988609932)) ;
#20300 = CARTESIAN_POINT('Origin',(1.14863049153645,-0.95,-8.72471478008953)) ;
#20301 = CARTESIAN_POINT('',(0.998630491536451,-1.,-8.72471478008953)) ;
#20302 = CARTESIAN_POINT('Origin',(1.14863049153645,-1.,-8.72471478008953)) ;
#20303 = CARTESIAN_POINT('',(0.998630491536451,-0.8,-8.72471478008953)) ;
#20304 = CARTESIAN_POINT('',(0.998630491536451,-0.95,-8.72471478008953)) ;
#20305 = CARTESIAN_POINT('Origin',(1.14863049153645,-0.8,-8.72471478008953)) ;
#20306 = CARTESIAN_POINT('Origin',(1.14863049153645,-0.8,-8.72471478008953)) ;
#20307 = CARTESIAN_POINT('Origin',(-1.14863049153645,-0.95,-8.72471478008953)) ;
#20308 = CARTESIAN_POINT('',(-1.29863049153645,-1.,-8.72471478008953)) ;
#20309 = CARTESIAN_POINT('Origin',(-1.14863049153645,-1.,-8.72471478008953)) ;
#20310 = CARTESIAN_POINT('',(-1.29863049153645,-0.8,-8.72471478008953)) ;
#20311 = CARTESIAN_POINT('',(-1.29863049153645,-0.95,-8.72471478008953)) ;
#20312 = CARTESIAN_POINT('Origin',(-1.14863049153645,-0.8,-8.72471478008953)) ;
#20313 = CARTESIAN_POINT('Origin',(-1.14863049153645,-0.8,-8.72471478008953)) ;
#20314 = CARTESIAN_POINT('Origin',(-3.36761420481279,-0.95,-8.13013988609933)) ;
#20315 = CARTESIAN_POINT('',(-3.51761420481279,-1.,-8.13013988609933)) ;
#20316 = CARTESIAN_POINT('Origin',(-3.36761420481279,-1.,-8.13013988609933)) ;
#20317 = CARTESIAN_POINT('',(-3.51761420481279,-0.8,-8.13013988609933)) ;
#20318 = CARTESIAN_POINT('',(-3.51761420481279,-0.95,-8.13013988609933)) ;
#20319 = CARTESIAN_POINT('Origin',(-3.36761420481279,-0.8,-8.13013988609933)) ;
#20320 = CARTESIAN_POINT('Origin',(-3.36761420481279,-0.8,-8.13013988609933)) ;
#20321 = CARTESIAN_POINT('Origin',(-5.35710057527674,-0.95,-6.98150939456287)) ;
#20322 = CARTESIAN_POINT('',(-5.50710057527674,-1.,-6.98150939456287)) ;
#20323 = CARTESIAN_POINT('Origin',(-5.35710057527674,-1.,-6.98150939456287)) ;
#20324 = CARTESIAN_POINT('',(-5.50710057527674,-0.8,-6.98150939456287)) ;
#20325 = CARTESIAN_POINT('',(-5.50710057527674,-0.95,-6.98150939456287)) ;
#20326 = CARTESIAN_POINT('Origin',(-5.35710057527674,-0.8,-6.98150939456287)) ;
#20327 = CARTESIAN_POINT('Origin',(-5.35710057527674,-0.8,-6.98150939456287)) ;
#20328 = CARTESIAN_POINT('Origin',(-6.98150939456287,-0.95,-5.35710057527674)) ;
#20329 = CARTESIAN_POINT('',(-7.13150939456287,-1.,-5.35710057527674)) ;
#20330 = CARTESIAN_POINT('Origin',(-6.98150939456287,-1.,-5.35710057527674)) ;
#20331 = CARTESIAN_POINT('',(-7.13150939456287,-0.8,-5.35710057527674)) ;
#20332 = CARTESIAN_POINT('',(-7.13150939456287,-0.95,-5.35710057527674)) ;
#20333 = CARTESIAN_POINT('Origin',(-6.98150939456287,-0.8,-5.35710057527674)) ;
#20334 = CARTESIAN_POINT('Origin',(-6.98150939456287,-0.8,-5.35710057527674)) ;
#20335 = CARTESIAN_POINT('Origin',(-8.13013988609933,-0.95,-3.36761420481279)) ;
#20336 = CARTESIAN_POINT('',(-8.28013988609933,-1.,-3.36761420481279)) ;
#20337 = CARTESIAN_POINT('Origin',(-8.13013988609933,-1.,-3.36761420481279)) ;
#20338 = CARTESIAN_POINT('',(-8.28013988609933,-0.8,-3.36761420481279)) ;
#20339 = CARTESIAN_POINT('',(-8.28013988609933,-0.95,-3.36761420481279)) ;
#20340 = CARTESIAN_POINT('Origin',(-8.13013988609933,-0.8,-3.36761420481279)) ;
#20341 = CARTESIAN_POINT('Origin',(-8.13013988609933,-0.8,-3.36761420481279)) ;
#20342 = CARTESIAN_POINT('Origin',(-8.72471478008953,-0.95,-1.14863049153645)) ;
#20343 = CARTESIAN_POINT('',(-8.87471478008953,-1.,-1.14863049153645)) ;
#20344 = CARTESIAN_POINT('Origin',(-8.72471478008953,-1.,-1.14863049153645)) ;
#20345 = CARTESIAN_POINT('',(-8.87471478008953,-0.8,-1.14863049153645)) ;
#20346 = CARTESIAN_POINT('',(-8.87471478008953,-0.95,-1.14863049153645)) ;
#20347 = CARTESIAN_POINT('Origin',(-8.72471478008953,-0.8,-1.14863049153645)) ;
#20348 = CARTESIAN_POINT('Origin',(-8.72471478008953,-0.8,-1.14863049153645)) ;
#20349 = CARTESIAN_POINT('Origin',(-8.72471478008953,-0.95,1.14863049153645)) ;
#20350 = CARTESIAN_POINT('',(-8.87471478008953,-1.,1.14863049153645)) ;
#20351 = CARTESIAN_POINT('Origin',(-8.72471478008953,-1.,1.14863049153645)) ;
#20352 = CARTESIAN_POINT('',(-8.87471478008953,-0.8,1.14863049153645)) ;
#20353 = CARTESIAN_POINT('',(-8.87471478008953,-0.95,1.14863049153645)) ;
#20354 = CARTESIAN_POINT('Origin',(-8.72471478008953,-0.8,1.14863049153645)) ;
#20355 = CARTESIAN_POINT('Origin',(-8.72471478008953,-0.8,1.14863049153645)) ;
#20356 = CARTESIAN_POINT('Origin',(-8.13013988609932,-0.95,3.36761420481279)) ;
#20357 = CARTESIAN_POINT('',(-8.28013988609932,-1.,3.36761420481279)) ;
#20358 = CARTESIAN_POINT('Origin',(-8.13013988609932,-1.,3.36761420481279)) ;
#20359 = CARTESIAN_POINT('',(-8.28013988609932,-0.8,3.36761420481279)) ;
#20360 = CARTESIAN_POINT('',(-8.28013988609932,-0.95,3.36761420481279)) ;
#20361 = CARTESIAN_POINT('Origin',(-8.13013988609932,-0.8,3.36761420481279)) ;
#20362 = CARTESIAN_POINT('Origin',(-8.13013988609932,-0.8,3.36761420481279)) ;
#20363 = CARTESIAN_POINT('Origin',(-6.98150939456287,-0.95,5.35710057527674)) ;
#20364 = CARTESIAN_POINT('',(-7.13150939456287,-1.,5.35710057527674)) ;
#20365 = CARTESIAN_POINT('Origin',(-6.98150939456287,-1.,5.35710057527674)) ;
#20366 = CARTESIAN_POINT('',(-7.13150939456287,-0.8,5.35710057527674)) ;
#20367 = CARTESIAN_POINT('',(-7.13150939456287,-0.95,5.35710057527674)) ;
#20368 = CARTESIAN_POINT('Origin',(-6.98150939456287,-0.8,5.35710057527674)) ;
#20369 = CARTESIAN_POINT('Origin',(-6.98150939456287,-0.8,5.35710057527674)) ;
#20370 = CARTESIAN_POINT('Origin',(-5.35710057527674,-0.95,6.98150939456287)) ;
#20371 = CARTESIAN_POINT('',(-5.50710057527674,-1.,6.98150939456287)) ;
#20372 = CARTESIAN_POINT('Origin',(-5.35710057527674,-1.,6.98150939456287)) ;
#20373 = CARTESIAN_POINT('',(-5.50710057527674,-0.8,6.98150939456287)) ;
#20374 = CARTESIAN_POINT('',(-5.50710057527674,-0.95,6.98150939456287)) ;
#20375 = CARTESIAN_POINT('Origin',(-5.35710057527674,-0.8,6.98150939456287)) ;
#20376 = CARTESIAN_POINT('Origin',(-5.35710057527674,-0.8,6.98150939456287)) ;
#20377 = CARTESIAN_POINT('Origin',(-3.36761420481279,-0.95,8.13013988609932)) ;
#20378 = CARTESIAN_POINT('',(-3.51761420481279,-1.,8.13013988609932)) ;
#20379 = CARTESIAN_POINT('Origin',(-3.36761420481279,-1.,8.13013988609932)) ;
#20380 = CARTESIAN_POINT('',(-3.51761420481279,-0.8,8.13013988609932)) ;
#20381 = CARTESIAN_POINT('',(-3.51761420481279,-0.95,8.13013988609932)) ;
#20382 = CARTESIAN_POINT('Origin',(-3.36761420481279,-0.8,8.13013988609932)) ;
#20383 = CARTESIAN_POINT('Origin',(-3.36761420481279,-0.8,8.13013988609932)) ;
#20384 = CARTESIAN_POINT('Origin',(-1.14863049153645,-0.95,8.72471478008953)) ;
#20385 = CARTESIAN_POINT('',(-1.29863049153645,-1.,8.72471478008953)) ;
#20386 = CARTESIAN_POINT('Origin',(-1.14863049153645,-1.,8.72471478008953)) ;
#20387 = CARTESIAN_POINT('',(-1.29863049153645,-0.8,8.72471478008953)) ;
#20388 = CARTESIAN_POINT('',(-1.29863049153645,-0.95,8.72471478008953)) ;
#20389 = CARTESIAN_POINT('Origin',(-1.14863049153645,-0.8,8.72471478008953)) ;
#20390 = CARTESIAN_POINT('Origin',(-1.14863049153645,-0.8,8.72471478008953)) ;
#20391 = CARTESIAN_POINT('Origin',(1.14863049153646,-0.95,8.72471478008953)) ;
#20392 = CARTESIAN_POINT('',(0.998630491536455,-1.,8.72471478008953)) ;
#20393 = CARTESIAN_POINT('Origin',(1.14863049153646,-1.,8.72471478008953)) ;
#20394 = CARTESIAN_POINT('',(0.998630491536455,-0.8,8.72471478008953)) ;
#20395 = CARTESIAN_POINT('',(0.998630491536455,-0.95,8.72471478008953)) ;
#20396 = CARTESIAN_POINT('Origin',(1.14863049153646,-0.8,8.72471478008953)) ;
#20397 = CARTESIAN_POINT('Origin',(1.14863049153646,-0.8,8.72471478008953)) ;
#20398 = CARTESIAN_POINT('Origin',(3.36761420481279,-0.95,8.13013988609932)) ;
#20399 = CARTESIAN_POINT('',(3.21761420481279,-1.,8.13013988609932)) ;
#20400 = CARTESIAN_POINT('Origin',(3.36761420481279,-1.,8.13013988609932)) ;
#20401 = CARTESIAN_POINT('',(3.21761420481279,-0.8,8.13013988609932)) ;
#20402 = CARTESIAN_POINT('',(3.21761420481279,-0.95,8.13013988609932)) ;
#20403 = CARTESIAN_POINT('Origin',(3.36761420481279,-0.8,8.13013988609932)) ;
#20404 = CARTESIAN_POINT('Origin',(3.36761420481279,-0.8,8.13013988609932)) ;
#20405 = CARTESIAN_POINT('Origin',(5.35710057527674,-0.95,6.98150939456287)) ;
#20406 = CARTESIAN_POINT('',(5.20710057527674,-1.,6.98150939456287)) ;
#20407 = CARTESIAN_POINT('Origin',(5.35710057527674,-1.,6.98150939456287)) ;
#20408 = CARTESIAN_POINT('',(5.20710057527674,-0.8,6.98150939456287)) ;
#20409 = CARTESIAN_POINT('',(5.20710057527674,-0.95,6.98150939456287)) ;
#20410 = CARTESIAN_POINT('Origin',(5.35710057527674,-0.8,6.98150939456287)) ;
#20411 = CARTESIAN_POINT('Origin',(5.35710057527674,-0.8,6.98150939456287)) ;
#20412 = CARTESIAN_POINT('Origin',(6.98150939456287,-0.95,5.35710057527674)) ;
#20413 = CARTESIAN_POINT('',(6.83150939456287,-1.,5.35710057527674)) ;
#20414 = CARTESIAN_POINT('Origin',(6.98150939456287,-1.,5.35710057527674)) ;
#20415 = CARTESIAN_POINT('',(6.83150939456287,-0.8,5.35710057527674)) ;
#20416 = CARTESIAN_POINT('',(6.83150939456287,-0.95,5.35710057527674)) ;
#20417 = CARTESIAN_POINT('Origin',(6.98150939456287,-0.8,5.35710057527674)) ;
#20418 = CARTESIAN_POINT('Origin',(6.98150939456287,-0.8,5.35710057527674)) ;
#20419 = CARTESIAN_POINT('Origin',(8.13013988609932,-0.95,3.36761420481279)) ;
#20420 = CARTESIAN_POINT('',(7.98013988609932,-1.,3.36761420481279)) ;
#20421 = CARTESIAN_POINT('Origin',(8.13013988609932,-1.,3.36761420481279)) ;
#20422 = CARTESIAN_POINT('',(7.98013988609932,-0.8,3.36761420481279)) ;
#20423 = CARTESIAN_POINT('',(7.98013988609932,-0.95,3.36761420481279)) ;
#20424 = CARTESIAN_POINT('Origin',(8.13013988609932,-0.8,3.36761420481279)) ;
#20425 = CARTESIAN_POINT('Origin',(8.13013988609932,-0.8,3.36761420481279)) ;
#20426 = CARTESIAN_POINT('Origin',(8.72471478008953,-0.95,1.14863049153645)) ;
#20427 = CARTESIAN_POINT('',(8.57471478008953,-1.,1.14863049153645)) ;
#20428 = CARTESIAN_POINT('Origin',(8.72471478008953,-1.,1.14863049153645)) ;
#20429 = CARTESIAN_POINT('',(8.57471478008953,-0.8,1.14863049153645)) ;
#20430 = CARTESIAN_POINT('',(8.57471478008953,-0.95,1.14863049153645)) ;
#20431 = CARTESIAN_POINT('Origin',(8.72471478008953,-0.8,1.14863049153645)) ;
#20432 = CARTESIAN_POINT('Origin',(8.72471478008953,-0.8,1.14863049153645)) ;
#20433 = CARTESIAN_POINT('Origin',(8.5001472713438,-0.65,-2.27760759690218)) ;
#20434 = CARTESIAN_POINT('',(8.1001472713438,-1.,-2.27760759690218)) ;
#20435 = CARTESIAN_POINT('Origin',(8.5001472713438,-1.,-2.27760759690218)) ;
#20436 = CARTESIAN_POINT('',(8.1001472713438,-0.3,-2.27760759690218)) ;
#20437 = CARTESIAN_POINT('',(8.1001472713438,-0.65,-2.27760759690218)) ;
#20438 = CARTESIAN_POINT('Origin',(8.5001472713438,-0.3,-2.27760759690218)) ;
#20439 = CARTESIAN_POINT('Origin',(7.62102355330306,-0.65,-4.4)) ;
#20440 = CARTESIAN_POINT('',(7.22102355330306,-1.,-4.4)) ;
#20441 = CARTESIAN_POINT('Origin',(7.62102355330306,-1.,-4.4)) ;
#20442 = CARTESIAN_POINT('',(7.22102355330306,-0.3,-4.4)) ;
#20443 = CARTESIAN_POINT('',(7.22102355330306,-0.65,-4.4)) ;
#20444 = CARTESIAN_POINT('Origin',(7.62102355330306,-0.3,-4.4)) ;
#20445 = CARTESIAN_POINT('Origin',(6.22253967444162,-0.65,-6.22253967444162)) ;
#20446 = CARTESIAN_POINT('',(5.82253967444162,-1.,-6.22253967444162)) ;
#20447 = CARTESIAN_POINT('Origin',(6.22253967444162,-1.,-6.22253967444162)) ;
#20448 = CARTESIAN_POINT('',(5.82253967444162,-0.3,-6.22253967444162)) ;
#20449 = CARTESIAN_POINT('',(5.82253967444162,-0.65,-6.22253967444162)) ;
#20450 = CARTESIAN_POINT('Origin',(6.22253967444162,-0.3,-6.22253967444162)) ;
#20451 = CARTESIAN_POINT('Origin',(4.4,-0.65,-7.62102355330306)) ;
#20452 = CARTESIAN_POINT('',(4.,-1.,-7.62102355330306)) ;
#20453 = CARTESIAN_POINT('Origin',(4.4,-1.,-7.62102355330306)) ;
#20454 = CARTESIAN_POINT('',(4.,-0.3,-7.62102355330306)) ;
#20455 = CARTESIAN_POINT('',(4.,-0.65,-7.62102355330306)) ;
#20456 = CARTESIAN_POINT('Origin',(4.4,-0.3,-7.62102355330306)) ;
#20457 = CARTESIAN_POINT('Origin',(2.27760759690218,-0.65,-8.5001472713438)) ;
#20458 = CARTESIAN_POINT('',(1.87760759690218,-1.,-8.5001472713438)) ;
#20459 = CARTESIAN_POINT('Origin',(2.27760759690218,-1.,-8.5001472713438)) ;
#20460 = CARTESIAN_POINT('',(1.87760759690218,-0.3,-8.5001472713438)) ;
#20461 = CARTESIAN_POINT('',(1.87760759690218,-0.65,-8.5001472713438)) ;
#20462 = CARTESIAN_POINT('Origin',(2.27760759690218,-0.3,-8.5001472713438)) ;
#20463 = CARTESIAN_POINT('Origin',(-1.61653377487451E-15,-0.65,-8.8)) ;
#20464 = CARTESIAN_POINT('',(-0.400000000000002,-1.,-8.8)) ;
#20465 = CARTESIAN_POINT('Origin',(-1.61653377487451E-15,-1.,-8.8)) ;
#20466 = CARTESIAN_POINT('',(-0.400000000000002,-0.3,-8.8)) ;
#20467 = CARTESIAN_POINT('',(-0.400000000000002,-0.65,-8.8)) ;
#20468 = CARTESIAN_POINT('Origin',(-1.61653377487451E-15,-0.3,-8.8)) ;
#20469 = CARTESIAN_POINT('Origin',(-2.27760759690218,-0.65,-8.5001472713438)) ;
#20470 = CARTESIAN_POINT('',(-2.67760759690218,-1.,-8.5001472713438)) ;
#20471 = CARTESIAN_POINT('Origin',(-2.27760759690218,-1.,-8.5001472713438)) ;
#20472 = CARTESIAN_POINT('',(-2.67760759690218,-0.3,-8.5001472713438)) ;
#20473 = CARTESIAN_POINT('',(-2.67760759690218,-0.65,-8.5001472713438)) ;
#20474 = CARTESIAN_POINT('Origin',(-2.27760759690218,-0.3,-8.5001472713438)) ;
#20475 = CARTESIAN_POINT('Origin',(-4.4,-0.65,-7.62102355330306)) ;
#20476 = CARTESIAN_POINT('',(-4.80000000000001,-1.,-7.62102355330306)) ;
#20477 = CARTESIAN_POINT('Origin',(-4.4,-1.,-7.62102355330306)) ;
#20478 = CARTESIAN_POINT('',(-4.80000000000001,-0.3,-7.62102355330306)) ;
#20479 = CARTESIAN_POINT('',(-4.80000000000001,-0.65,-7.62102355330306)) ;
#20480 = CARTESIAN_POINT('Origin',(-4.4,-0.3,-7.62102355330306)) ;
#20481 = CARTESIAN_POINT('Origin',(-6.22253967444162,-0.65,-6.22253967444162)) ;
#20482 = CARTESIAN_POINT('',(-6.62253967444162,-1.,-6.22253967444162)) ;
#20483 = CARTESIAN_POINT('Origin',(-6.22253967444162,-1.,-6.22253967444162)) ;
#20484 = CARTESIAN_POINT('',(-6.62253967444162,-0.3,-6.22253967444162)) ;
#20485 = CARTESIAN_POINT('',(-6.62253967444162,-0.65,-6.22253967444162)) ;
#20486 = CARTESIAN_POINT('Origin',(-6.22253967444162,-0.3,-6.22253967444162)) ;
#20487 = CARTESIAN_POINT('Origin',(-7.62102355330306,-0.65,-4.4)) ;
#20488 = CARTESIAN_POINT('',(-8.02102355330306,-1.,-4.4)) ;
#20489 = CARTESIAN_POINT('Origin',(-7.62102355330306,-1.,-4.4)) ;
#20490 = CARTESIAN_POINT('',(-8.02102355330306,-0.3,-4.4)) ;
#20491 = CARTESIAN_POINT('',(-8.02102355330306,-0.65,-4.4)) ;
#20492 = CARTESIAN_POINT('Origin',(-7.62102355330306,-0.3,-4.4)) ;
#20493 = CARTESIAN_POINT('Origin',(-8.5001472713438,-0.65,-2.27760759690218)) ;
#20494 = CARTESIAN_POINT('',(-8.9001472713438,-1.,-2.27760759690218)) ;
#20495 = CARTESIAN_POINT('Origin',(-8.5001472713438,-1.,-2.27760759690218)) ;
#20496 = CARTESIAN_POINT('',(-8.9001472713438,-0.3,-2.27760759690218)) ;
#20497 = CARTESIAN_POINT('',(-8.9001472713438,-0.65,-2.27760759690218)) ;
#20498 = CARTESIAN_POINT('Origin',(-8.5001472713438,-0.3,-2.27760759690218)) ;
#20499 = CARTESIAN_POINT('Origin',(-8.8,-0.65,1.07768918324967E-15)) ;
#20500 = CARTESIAN_POINT('',(-9.2,-1.,1.12667505521557E-15)) ;
#20501 = CARTESIAN_POINT('Origin',(-8.8,-1.,1.07768918324967E-15)) ;
#20502 = CARTESIAN_POINT('',(-9.2,-0.3,1.02870331128378E-15)) ;
#20503 = CARTESIAN_POINT('',(-9.2,-0.65,1.12667505521557E-15)) ;
#20504 = CARTESIAN_POINT('Origin',(-8.8,-0.3,1.07768918324967E-15)) ;
#20505 = CARTESIAN_POINT('Origin',(-8.5001472713438,-0.65,2.27760759690219)) ;
#20506 = CARTESIAN_POINT('',(-8.9001472713438,-1.,2.27760759690219)) ;
#20507 = CARTESIAN_POINT('Origin',(-8.5001472713438,-1.,2.27760759690219)) ;
#20508 = CARTESIAN_POINT('',(-8.9001472713438,-0.3,2.27760759690219)) ;
#20509 = CARTESIAN_POINT('',(-8.9001472713438,-0.65,2.27760759690219)) ;
#20510 = CARTESIAN_POINT('Origin',(-8.5001472713438,-0.3,2.27760759690219)) ;
#20511 = CARTESIAN_POINT('Origin',(-7.62102355330306,-0.65,4.4)) ;
#20512 = CARTESIAN_POINT('',(-8.02102355330306,-1.,4.4)) ;
#20513 = CARTESIAN_POINT('Origin',(-7.62102355330306,-1.,4.4)) ;
#20514 = CARTESIAN_POINT('',(-8.02102355330306,-0.3,4.4)) ;
#20515 = CARTESIAN_POINT('',(-8.02102355330306,-0.65,4.4)) ;
#20516 = CARTESIAN_POINT('Origin',(-7.62102355330306,-0.3,4.4)) ;
#20517 = CARTESIAN_POINT('Origin',(-6.22253967444162,-0.65,6.22253967444162)) ;
#20518 = CARTESIAN_POINT('',(-6.62253967444162,-1.,6.22253967444162)) ;
#20519 = CARTESIAN_POINT('Origin',(-6.22253967444162,-1.,6.22253967444162)) ;
#20520 = CARTESIAN_POINT('',(-6.62253967444162,-0.3,6.22253967444162)) ;
#20521 = CARTESIAN_POINT('',(-6.62253967444162,-0.65,6.22253967444162)) ;
#20522 = CARTESIAN_POINT('Origin',(-6.22253967444162,-0.3,6.22253967444162)) ;
#20523 = CARTESIAN_POINT('Origin',(-4.4,-0.65,7.62102355330306)) ;
#20524 = CARTESIAN_POINT('',(-4.8,-1.,7.62102355330306)) ;
#20525 = CARTESIAN_POINT('Origin',(-4.4,-1.,7.62102355330306)) ;
#20526 = CARTESIAN_POINT('',(-4.8,-0.3,7.62102355330306)) ;
#20527 = CARTESIAN_POINT('',(-4.8,-0.65,7.62102355330306)) ;
#20528 = CARTESIAN_POINT('Origin',(-4.4,-0.3,7.62102355330306)) ;
#20529 = CARTESIAN_POINT('Origin',(-2.27760759690218,-0.65,8.5001472713438)) ;
#20530 = CARTESIAN_POINT('',(-2.67760759690218,-1.,8.5001472713438)) ;
#20531 = CARTESIAN_POINT('Origin',(-2.27760759690218,-1.,8.5001472713438)) ;
#20532 = CARTESIAN_POINT('',(-2.67760759690218,-0.3,8.5001472713438)) ;
#20533 = CARTESIAN_POINT('',(-2.67760759690218,-0.65,8.5001472713438)) ;
#20534 = CARTESIAN_POINT('Origin',(-2.27760759690218,-0.3,8.5001472713438)) ;
#20535 = CARTESIAN_POINT('Origin',(5.38844591624835E-16,-0.65,8.8)) ;
#20536 = CARTESIAN_POINT('',(-0.399999999999999,-1.,8.8)) ;
#20537 = CARTESIAN_POINT('Origin',(5.38844591624835E-16,-1.,8.8)) ;
#20538 = CARTESIAN_POINT('',(-0.399999999999999,-0.3,8.8)) ;
#20539 = CARTESIAN_POINT('',(-0.399999999999999,-0.65,8.8)) ;
#20540 = CARTESIAN_POINT('Origin',(5.38844591624835E-16,-0.3,8.8)) ;
#20541 = CARTESIAN_POINT('Origin',(2.27760759690218,-0.65,8.5001472713438)) ;
#20542 = CARTESIAN_POINT('',(1.87760759690218,-1.,8.5001472713438)) ;
#20543 = CARTESIAN_POINT('Origin',(2.27760759690218,-1.,8.5001472713438)) ;
#20544 = CARTESIAN_POINT('',(1.87760759690218,-0.3,8.5001472713438)) ;
#20545 = CARTESIAN_POINT('',(1.87760759690218,-0.65,8.5001472713438)) ;
#20546 = CARTESIAN_POINT('Origin',(2.27760759690218,-0.3,8.5001472713438)) ;
#20547 = CARTESIAN_POINT('Origin',(4.4,-0.65,7.62102355330306)) ;
#20548 = CARTESIAN_POINT('',(4.,-1.,7.62102355330306)) ;
#20549 = CARTESIAN_POINT('Origin',(4.4,-1.,7.62102355330306)) ;
#20550 = CARTESIAN_POINT('',(4.,-0.3,7.62102355330306)) ;
#20551 = CARTESIAN_POINT('',(4.,-0.65,7.62102355330306)) ;
#20552 = CARTESIAN_POINT('Origin',(4.4,-0.3,7.62102355330306)) ;
#20553 = CARTESIAN_POINT('Origin',(6.22253967444162,-0.65,6.22253967444162)) ;
#20554 = CARTESIAN_POINT('',(5.82253967444162,-1.,6.22253967444162)) ;
#20555 = CARTESIAN_POINT('Origin',(6.22253967444162,-1.,6.22253967444162)) ;
#20556 = CARTESIAN_POINT('',(5.82253967444162,-0.3,6.22253967444162)) ;
#20557 = CARTESIAN_POINT('',(5.82253967444162,-0.65,6.22253967444162)) ;
#20558 = CARTESIAN_POINT('Origin',(6.22253967444162,-0.3,6.22253967444162)) ;
#20559 = CARTESIAN_POINT('Origin',(7.62102355330306,-0.65,4.4)) ;
#20560 = CARTESIAN_POINT('',(7.22102355330306,-1.,4.4)) ;
#20561 = CARTESIAN_POINT('Origin',(7.62102355330306,-1.,4.4)) ;
#20562 = CARTESIAN_POINT('',(7.22102355330306,-0.3,4.4)) ;
#20563 = CARTESIAN_POINT('',(7.22102355330306,-0.65,4.4)) ;
#20564 = CARTESIAN_POINT('Origin',(7.62102355330306,-0.3,4.4)) ;
#20565 = CARTESIAN_POINT('Origin',(8.5001472713438,-0.65,2.27760759690218)) ;
#20566 = CARTESIAN_POINT('',(8.1001472713438,-1.,2.27760759690218)) ;
#20567 = CARTESIAN_POINT('Origin',(8.5001472713438,-1.,2.27760759690218)) ;
#20568 = CARTESIAN_POINT('',(8.1001472713438,-0.3,2.27760759690218)) ;
#20569 = CARTESIAN_POINT('',(8.1001472713438,-0.65,2.27760759690218)) ;
#20570 = CARTESIAN_POINT('Origin',(8.5001472713438,-0.3,2.27760759690218)) ;
#20571 = CARTESIAN_POINT('Origin',(8.8,-0.65,0.)) ;
#20572 = CARTESIAN_POINT('',(8.4,-1.,4.89858719658941E-17)) ;
#20573 = CARTESIAN_POINT('Origin',(8.8,-1.,0.)) ;
#20574 = CARTESIAN_POINT('',(8.4,-0.3,-4.89858719658941E-17)) ;
#20575 = CARTESIAN_POINT('',(8.4,-0.65,4.89858719658941E-17)) ;
#20576 = CARTESIAN_POINT('Origin',(8.8,-0.3,0.)) ;
#20577 = CARTESIAN_POINT('Origin',(1.55884572681199,-0.65,-0.900000000000001)) ;
#20578 = CARTESIAN_POINT('',(1.34384572681199,-1.,-0.900000000000001)) ;
#20579 = CARTESIAN_POINT('Origin',(1.55884572681199,-1.,-0.900000000000001)) ;
#20580 = CARTESIAN_POINT('',(1.34384572681199,-0.3,-0.900000000000001)) ;
#20581 = CARTESIAN_POINT('',(1.34384572681199,-0.65,-0.900000000000001)) ;
#20582 = CARTESIAN_POINT('Origin',(1.55884572681199,-0.3,-0.900000000000001)) ;
#20583 = CARTESIAN_POINT('Origin',(-1.55884572681199,-0.65,-0.9)) ;
#20584 = CARTESIAN_POINT('',(-1.77384572681199,-1.,-0.9)) ;
#20585 = CARTESIAN_POINT('Origin',(-1.55884572681199,-1.,-0.9)) ;
#20586 = CARTESIAN_POINT('',(-1.77384572681199,-0.3,-0.9)) ;
#20587 = CARTESIAN_POINT('',(-1.77384572681199,-0.65,-0.9)) ;
#20588 = CARTESIAN_POINT('Origin',(-1.55884572681199,-0.3,-0.9)) ;
#20589 = CARTESIAN_POINT('Origin',(1.10218211923262E-16,-0.65,1.8)) ;
#20590 = CARTESIAN_POINT('',(-0.215,-1.,1.8)) ;
#20591 = CARTESIAN_POINT('Origin',(1.10218211923262E-16,-1.,1.8)) ;
#20592 = CARTESIAN_POINT('',(-0.215,-0.3,1.8)) ;
#20593 = CARTESIAN_POINT('',(-0.215,-0.65,1.8)) ;
#20594 = CARTESIAN_POINT('Origin',(1.10218211923262E-16,-0.3,1.8)) ;
#20595 = CARTESIAN_POINT('Origin',(0.,-0.65,0.)) ;
#20596 = CARTESIAN_POINT('',(-0.51,-1.,6.2456986756515E-17)) ;
#20597 = CARTESIAN_POINT('Origin',(0.,-1.,0.)) ;
#20598 = CARTESIAN_POINT('',(-0.51,-0.3,-6.2456986756515E-17)) ;
#20599 = CARTESIAN_POINT('',(-0.51,-0.65,6.2456986756515E-17)) ;
#20600 = CARTESIAN_POINT('Origin',(0.,-0.3,0.)) ;
#20601 = CARTESIAN_POINT('Origin',(0.,-0.65,0.)) ;
#20602 = CARTESIAN_POINT('',(-10.,-0.3,1.22464679914735E-15)) ;
#20603 = CARTESIAN_POINT('Origin',(0.,-0.3,0.)) ;
#20604 = CARTESIAN_POINT('',(-10.,-1.,1.22464679914735E-15)) ;
#20605 = CARTESIAN_POINT('',(-10.,-0.65,1.22464679914735E-15)) ;
#20606 = CARTESIAN_POINT('Origin',(0.,-1.,0.)) ;
#20607 = CARTESIAN_POINT('Origin',(0.,-1.,0.)) ;
#20608 = CARTESIAN_POINT('Origin',(0.,-0.3,0.)) ;
#20609 = CARTESIAN_POINT('',(0.,0.,0.)) ;
#20610 = CARTESIAN_POINT('Origin',(0.,-4.08,0.)) ;
#20611 = CARTESIAN_POINT('',(-1.45,-4.08,1.77573785876366E-16)) ;
#20612 = CARTESIAN_POINT('Origin',(0.,-4.08,0.)) ;
#20613 = CARTESIAN_POINT('',(-1.05,-4.08,-1.28587913910472E-16)) ;
#20614 = CARTESIAN_POINT('Origin',(0.,-4.08,0.)) ;
#20615 = CARTESIAN_POINT('Origin',(0.,-5.02,0.)) ;
#20616 = CARTESIAN_POINT('',(-1.45,-5.02,-1.77573785876366E-16)) ;
#20617 = CARTESIAN_POINT('Origin',(0.,-5.02,0.)) ;
#20618 = CARTESIAN_POINT('',(-1.05,-5.02,1.28587913910472E-16)) ;
#20619 = CARTESIAN_POINT('Origin',(0.,-5.02,0.)) ;
#20620 = CARTESIAN_POINT('Origin',(0.,-4.55,0.)) ;
#20621 = CARTESIAN_POINT('',(-1.05,-4.55,1.28587913910472E-16)) ;
#20622 = CARTESIAN_POINT('Origin',(0.,-4.55,0.)) ;
#20623 = CARTESIAN_POINT('',(-1.45,-4.55,1.77573785876366E-16)) ;
#20624 = CARTESIAN_POINT('Origin',(0.,-5.1,0.)) ;
#20625 = CARTESIAN_POINT('',(-1.75,-5.1,2.14313189850787E-16)) ;
#20626 = CARTESIAN_POINT('Origin',(0.,-5.1,0.)) ;
#20627 = CARTESIAN_POINT('',(-0.75,-5.1,9.18485099360515E-17)) ;
#20628 = CARTESIAN_POINT('Origin',(0.,-5.1,0.)) ;
#20629 = CARTESIAN_POINT('Origin',(0.,-4.55,0.)) ;
#20630 = CARTESIAN_POINT('',(-1.75,-4.,2.14313189850787E-16)) ;
#20631 = CARTESIAN_POINT('Origin',(0.,-4.,0.)) ;
#20632 = CARTESIAN_POINT('',(-1.75,-4.55,2.14313189850787E-16)) ;
#20633 = CARTESIAN_POINT('Origin',(0.,-4.,0.)) ;
#20634 = CARTESIAN_POINT('',(-0.75,-4.,-9.18485099360515E-17)) ;
#20635 = CARTESIAN_POINT('Origin',(0.,-4.,0.)) ;
#20636 = CARTESIAN_POINT('Origin',(0.,-4.55,0.)) ;
#20637 = CARTESIAN_POINT('',(-0.75,-4.55,9.18485099360515E-17)) ;
#20638 = CARTESIAN_POINT('',(0.,0.,0.)) ;
#20639 = CARTESIAN_POINT('Origin',(0.,-2.58,0.)) ;
#20640 = CARTESIAN_POINT('',(-1.45,-2.58,1.77573785876366E-16)) ;
#20641 = CARTESIAN_POINT('Origin',(0.,-2.58,0.)) ;
#20642 = CARTESIAN_POINT('',(-1.05,-2.58,-1.28587913910472E-16)) ;
#20643 = CARTESIAN_POINT('Origin',(0.,-2.58,0.)) ;
#20644 = CARTESIAN_POINT('Origin',(0.,-3.52,0.)) ;
#20645 = CARTESIAN_POINT('',(-1.45,-3.52,-1.77573785876366E-16)) ;
#20646 = CARTESIAN_POINT('Origin',(0.,-3.52,0.)) ;
#20647 = CARTESIAN_POINT('',(-1.05,-3.52,1.28587913910472E-16)) ;
#20648 = CARTESIAN_POINT('Origin',(0.,-3.52,0.)) ;
#20649 = CARTESIAN_POINT('Origin',(0.,-3.05,0.)) ;
#20650 = CARTESIAN_POINT('',(-1.05,-3.05,1.28587913910472E-16)) ;
#20651 = CARTESIAN_POINT('Origin',(0.,-3.05,0.)) ;
#20652 = CARTESIAN_POINT('',(-1.45,-3.05,1.77573785876366E-16)) ;
#20653 = CARTESIAN_POINT('Origin',(0.,-3.6,0.)) ;
#20654 = CARTESIAN_POINT('',(-1.75,-3.6,2.14313189850787E-16)) ;
#20655 = CARTESIAN_POINT('Origin',(0.,-3.6,0.)) ;
#20656 = CARTESIAN_POINT('',(-0.75,-3.6,9.18485099360515E-17)) ;
#20657 = CARTESIAN_POINT('Origin',(0.,-3.6,0.)) ;
#20658 = CARTESIAN_POINT('Origin',(0.,-3.05,0.)) ;
#20659 = CARTESIAN_POINT('',(-1.75,-2.5,2.14313189850787E-16)) ;
#20660 = CARTESIAN_POINT('Origin',(0.,-2.5,0.)) ;
#20661 = CARTESIAN_POINT('',(-1.75,-3.05,2.14313189850787E-16)) ;
#20662 = CARTESIAN_POINT('Origin',(0.,-2.5,0.)) ;
#20663 = CARTESIAN_POINT('',(-0.75,-2.5,-9.18485099360515E-17)) ;
#20664 = CARTESIAN_POINT('Origin',(0.,-2.5,0.)) ;
#20665 = CARTESIAN_POINT('Origin',(0.,-3.05,0.)) ;
#20666 = CARTESIAN_POINT('',(-0.75,-3.05,9.18485099360515E-17)) ;
#20667 = CARTESIAN_POINT('',(0.,0.,0.)) ;
#20668 = CARTESIAN_POINT('Origin',(0.,-3.8,0.)) ;
#20669 = CARTESIAN_POINT('',(-0.75,-4.,9.18485099360515E-17)) ;
#20670 = CARTESIAN_POINT('Origin',(0.,-4.,0.)) ;
#20671 = CARTESIAN_POINT('',(-0.75,-3.6,-9.18485099360515E-17)) ;
#20672 = CARTESIAN_POINT('',(-0.75,-3.8,9.18485099360515E-17)) ;
#20673 = CARTESIAN_POINT('Origin',(0.,-3.6,0.)) ;
#20674 = CARTESIAN_POINT('Origin',(0.,-3.8,0.)) ;
#20675 = CARTESIAN_POINT('',(-1.1,-3.6,1.34711147906209E-16)) ;
#20676 = CARTESIAN_POINT('Origin',(0.,-3.6,0.)) ;
#20677 = CARTESIAN_POINT('',(-1.1,-4.,1.34711147906209E-16)) ;
#20678 = CARTESIAN_POINT('',(-1.1,-3.8,1.34711147906209E-16)) ;
#20679 = CARTESIAN_POINT('Origin',(0.,-4.,0.)) ;
#20680 = CARTESIAN_POINT('Origin',(0.,-4.,0.)) ;
#20681 = CARTESIAN_POINT('Origin',(0.,-3.6,0.)) ;
#20682 = CARTESIAN_POINT('',(0.,0.,0.)) ;
#20683 = CARTESIAN_POINT('Origin',(-0.2,-5.25,-0.8)) ;
#20684 = CARTESIAN_POINT('',(-0.2,-5.2,-0.928708781050335)) ;
#20685 = CARTESIAN_POINT('',(-0.2,-5.3,-0.928708781050335)) ;
#20686 = CARTESIAN_POINT('',(-0.2,-5.25,-0.928708781050335)) ;
#20687 = CARTESIAN_POINT('',(-0.2,-5.2,-0.676036241632059)) ;
#20688 = CARTESIAN_POINT('',(-0.2,-5.2,-0.4)) ;
#20689 = CARTESIAN_POINT('',(-0.2,-5.3,-0.676036241632059)) ;
#20690 = CARTESIAN_POINT('',(-0.2,-5.25,-0.676036241632059)) ;
#20691 = CARTESIAN_POINT('',(-0.2,-5.3,-0.4)) ;
#20692 = CARTESIAN_POINT('Origin',(0.2,-5.25,-0.8)) ;
#20693 = CARTESIAN_POINT('',(0.2,-5.3,-0.928708781050335)) ;
#20694 = CARTESIAN_POINT('',(0.2,-5.2,-0.928708781050335)) ;
#20695 = CARTESIAN_POINT('',(0.2,-5.25,-0.928708781050335)) ;
#20696 = CARTESIAN_POINT('',(0.2,-5.3,-0.676036241632059)) ;
#20697 = CARTESIAN_POINT('',(0.2,-5.3,-0.4)) ;
#20698 = CARTESIAN_POINT('',(0.2,-5.2,-0.676036241632059)) ;
#20699 = CARTESIAN_POINT('',(0.2,-5.25,-0.676036241632059)) ;
#20700 = CARTESIAN_POINT('',(0.2,-5.2,-0.4)) ;
#20701 = CARTESIAN_POINT('Origin',(0.,-5.2,0.)) ;
#20702 = CARTESIAN_POINT('Origin',(0.,-5.2,0.)) ;
#20703 = CARTESIAN_POINT('Origin',(0.,-5.2,0.)) ;
#20704 = CARTESIAN_POINT('Origin',(0.,-5.25,0.)) ;
#20705 = CARTESIAN_POINT('Origin',(0.,-5.3,0.)) ;
#20706 = CARTESIAN_POINT('Origin',(0.,-5.25,0.)) ;
#20707 = CARTESIAN_POINT('Origin',(0.,-5.3,0.)) ;
#20708 = CARTESIAN_POINT('Origin',(0.,-5.3,0.)) ;
#20709 = CARTESIAN_POINT('',(0.,0.,0.)) ;
#20710 = CARTESIAN_POINT('Origin',(0.83,-6.25,0.252)) ;
#20711 = CARTESIAN_POINT('',(1.01,-5.7,0.252)) ;
#20712 = CARTESIAN_POINT('',(0.706396489232499,-5.7,0.252)) ;
#20713 = CARTESIAN_POINT('',(0.415,-5.7,0.252)) ;
#20714 = CARTESIAN_POINT('',(1.01,-6.8,0.252)) ;
#20715 = CARTESIAN_POINT('',(1.01,-6.25,0.252)) ;
#20716 = CARTESIAN_POINT('',(0.706396489232499,-6.8,0.252)) ;
#20717 = CARTESIAN_POINT('',(0.415,-6.8,0.252)) ;
#20718 = CARTESIAN_POINT('',(0.706396489232499,-6.25,0.252)) ;
#20719 = CARTESIAN_POINT('Origin',(0.83,-6.25,-0.252)) ;
#20720 = CARTESIAN_POINT('',(0.706396489232499,-5.7,-0.252)) ;
#20721 = CARTESIAN_POINT('',(1.01,-5.7,-0.252)) ;
#20722 = CARTESIAN_POINT('',(0.415,-5.7,-0.252)) ;
#20723 = CARTESIAN_POINT('',(0.706396489232499,-6.8,-0.252)) ;
#20724 = CARTESIAN_POINT('',(0.706396489232499,-6.25,-0.252)) ;
#20725 = CARTESIAN_POINT('',(1.01,-6.8,-0.252)) ;
#20726 = CARTESIAN_POINT('',(0.415,-6.8,-0.252)) ;
#20727 = CARTESIAN_POINT('',(1.01,-6.25,-0.252)) ;
#20728 = CARTESIAN_POINT('Origin',(1.01,-6.25,0.)) ;
#20729 = CARTESIAN_POINT('',(1.01,-5.7,0.)) ;
#20730 = CARTESIAN_POINT('',(1.01,-6.8,0.)) ;
#20731 = CARTESIAN_POINT('Origin',(0.,-6.8,0.)) ;
#20732 = CARTESIAN_POINT('',(-1.4,-6.8,1.71450551880629E-16)) ;
#20733 = CARTESIAN_POINT('Origin',(0.,-6.8,0.)) ;
#20734 = CARTESIAN_POINT('Origin',(0.,-6.8,0.)) ;
#20735 = CARTESIAN_POINT('Origin',(0.,-6.25,0.)) ;
#20736 = CARTESIAN_POINT('Origin',(0.,-5.7,0.)) ;
#20737 = CARTESIAN_POINT('Origin',(2.21326859021798,-6.05,-1.56650635094611)) ;
#20738 = CARTESIAN_POINT('',(2.02921099245176,-5.7,-1.46024064732939)) ;
#20739 = CARTESIAN_POINT('',(2.02921099245176,-6.4,-1.46024064732939)) ;
#20740 = CARTESIAN_POINT('',(2.02921099245176,-6.05,-1.46024064732939)) ;
#20741 = CARTESIAN_POINT('',(2.47307621135332,-5.7,-1.71650635094611)) ;
#20742 = CARTESIAN_POINT('',(2.21326859021798,-5.7,-1.56650635094611)) ;
#20743 = CARTESIAN_POINT('',(2.47307621135332,-6.4,-1.71650635094611)) ;
#20744 = CARTESIAN_POINT('',(2.47307621135332,-6.05,-1.71650635094611)) ;
#20745 = CARTESIAN_POINT('',(2.21326859021798,-6.4,-1.56650635094611)) ;
#20746 = CARTESIAN_POINT('Origin',(2.46326859021798,-6.05,-1.13349364905389)) ;
#20747 = CARTESIAN_POINT('',(2.27921099245176,-6.4,-1.02722794543717)) ;
#20748 = CARTESIAN_POINT('',(2.27921099245176,-5.7,-1.02722794543717)) ;
#20749 = CARTESIAN_POINT('',(2.27921099245176,-6.05,-1.02722794543717)) ;
#20750 = CARTESIAN_POINT('',(2.72307621135332,-6.4,-1.28349364905389)) ;
#20751 = CARTESIAN_POINT('',(2.46326859021798,-6.4,-1.13349364905389)) ;
#20752 = CARTESIAN_POINT('',(2.72307621135332,-5.7,-1.28349364905389)) ;
#20753 = CARTESIAN_POINT('',(2.72307621135332,-6.05,-1.28349364905389)) ;
#20754 = CARTESIAN_POINT('',(2.46326859021798,-5.7,-1.13349364905389)) ;
#20755 = CARTESIAN_POINT('Origin',(2.59807621135332,-6.05,-1.5)) ;
#20756 = CARTESIAN_POINT('',(2.59807621135332,-6.4,-1.5)) ;
#20757 = CARTESIAN_POINT('',(2.59807621135332,-5.7,-1.5)) ;
#20758 = CARTESIAN_POINT('Origin',(0.,-6.05,0.)) ;
#20759 = CARTESIAN_POINT('',(1.46024064732938,-6.4,-2.02921099245176)) ;
#20760 = CARTESIAN_POINT('Origin',(0.,-6.4,0.)) ;
#20761 = CARTESIAN_POINT('',(1.46024064732938,-5.7,-2.02921099245176)) ;
#20762 = CARTESIAN_POINT('',(1.46024064732938,-6.05,-2.02921099245176)) ;
#20763 = CARTESIAN_POINT('Origin',(0.,-5.7,0.)) ;
#20764 = CARTESIAN_POINT('Origin',(0.,-6.05,0.)) ;
#20765 = CARTESIAN_POINT('',(2.48746859276655,-5.7,-0.25)) ;
#20766 = CARTESIAN_POINT('Origin',(0.,-5.7,0.)) ;
#20767 = CARTESIAN_POINT('',(2.48746859276655,-6.4,-0.25)) ;
#20768 = CARTESIAN_POINT('',(2.48746859276655,-6.05,-0.25)) ;
#20769 = CARTESIAN_POINT('Origin',(0.,-6.4,0.)) ;
#20770 = CARTESIAN_POINT('Origin',(0.,-5.7,0.)) ;
#20771 = CARTESIAN_POINT('',(1.71650635094611,-5.7,-2.47307621135332)) ;
#20772 = CARTESIAN_POINT('',(1.56650635094611,-5.7,-2.21326859021798)) ;
#20773 = CARTESIAN_POINT('',(1.28349364905389,-5.7,-2.72307621135332)) ;
#20774 = CARTESIAN_POINT('',(1.5,-5.7,-2.59807621135332)) ;
#20775 = CARTESIAN_POINT('',(1.02722794543717,-5.7,-2.27921099245176)) ;
#20776 = CARTESIAN_POINT('',(1.13349364905389,-5.7,-2.46326859021798)) ;
#20777 = CARTESIAN_POINT('',(0.25,-5.7,-2.48746859276655)) ;
#20778 = CARTESIAN_POINT('Origin',(0.,-5.7,0.)) ;
#20779 = CARTESIAN_POINT('',(0.249999999999999,-5.7,-3.)) ;
#20780 = CARTESIAN_POINT('',(0.25,-5.7,-2.7)) ;
#20781 = CARTESIAN_POINT('',(-0.250000000000001,-5.7,-3.)) ;
#20782 = CARTESIAN_POINT('',(-5.51091059616309E-16,-5.7,-3.)) ;
#20783 = CARTESIAN_POINT('',(-0.25,-5.7,-2.48746859276655)) ;
#20784 = CARTESIAN_POINT('',(-0.25,-5.7,-2.7)) ;
#20785 = CARTESIAN_POINT('',(-1.02722794543717,-5.7,-2.27921099245176)) ;
#20786 = CARTESIAN_POINT('Origin',(0.,-5.7,0.)) ;
#20787 = CARTESIAN_POINT('',(-1.28349364905389,-5.7,-2.72307621135332)) ;
#20788 = CARTESIAN_POINT('',(-1.13349364905389,-5.7,-2.46326859021798)) ;
#20789 = CARTESIAN_POINT('',(-1.71650635094611,-5.7,-2.47307621135332)) ;
#20790 = CARTESIAN_POINT('',(-1.5,-5.7,-2.59807621135332)) ;
#20791 = CARTESIAN_POINT('',(-1.46024064732939,-5.7,-2.02921099245176)) ;
#20792 = CARTESIAN_POINT('',(-1.56650635094611,-5.7,-2.21326859021798)) ;
#20793 = CARTESIAN_POINT('',(-2.02921099245176,-5.7,-1.46024064732938)) ;
#20794 = CARTESIAN_POINT('Origin',(0.,-5.7,0.)) ;
#20795 = CARTESIAN_POINT('',(-2.47307621135332,-5.7,-1.71650635094611)) ;
#20796 = CARTESIAN_POINT('',(-2.21326859021798,-5.7,-1.56650635094611)) ;
#20797 = CARTESIAN_POINT('',(-2.72307621135332,-5.7,-1.28349364905389)) ;
#20798 = CARTESIAN_POINT('',(-2.59807621135332,-5.7,-1.5)) ;
#20799 = CARTESIAN_POINT('',(-2.27921099245176,-5.7,-1.02722794543717)) ;
#20800 = CARTESIAN_POINT('',(-2.46326859021798,-5.7,-1.13349364905389)) ;
#20801 = CARTESIAN_POINT('',(-2.48746859276655,-5.7,-0.25)) ;
#20802 = CARTESIAN_POINT('Origin',(0.,-5.7,0.)) ;
#20803 = CARTESIAN_POINT('',(-3.,-5.7,-0.25)) ;
#20804 = CARTESIAN_POINT('',(-2.7,-5.7,-0.25)) ;
#20805 = CARTESIAN_POINT('',(-3.,-5.7,0.25)) ;
#20806 = CARTESIAN_POINT('',(-3.,-5.7,3.67394039744206E-16)) ;
#20807 = CARTESIAN_POINT('',(-2.48746859276655,-5.7,0.25)) ;
#20808 = CARTESIAN_POINT('',(-2.7,-5.7,0.25)) ;
#20809 = CARTESIAN_POINT('',(-2.27921099245176,-5.7,1.02722794543716)) ;
#20810 = CARTESIAN_POINT('Origin',(0.,-5.7,0.)) ;
#20811 = CARTESIAN_POINT('',(-2.72307621135332,-5.7,1.28349364905389)) ;
#20812 = CARTESIAN_POINT('',(-2.46326859021798,-5.7,1.13349364905389)) ;
#20813 = CARTESIAN_POINT('',(-2.47307621135332,-5.7,1.71650635094611)) ;
#20814 = CARTESIAN_POINT('',(-2.59807621135332,-5.7,1.5)) ;
#20815 = CARTESIAN_POINT('',(-2.02921099245176,-5.7,1.46024064732938)) ;
#20816 = CARTESIAN_POINT('',(-2.21326859021798,-5.7,1.56650635094611)) ;
#20817 = CARTESIAN_POINT('',(-1.46024064732938,-5.7,2.02921099245176)) ;
#20818 = CARTESIAN_POINT('Origin',(0.,-5.7,0.)) ;
#20819 = CARTESIAN_POINT('',(-1.71650635094611,-5.7,2.47307621135332)) ;
#20820 = CARTESIAN_POINT('',(-1.56650635094611,-5.7,2.21326859021798)) ;
#20821 = CARTESIAN_POINT('',(-1.28349364905389,-5.7,2.72307621135332)) ;
#20822 = CARTESIAN_POINT('',(-1.5,-5.7,2.59807621135332)) ;
#20823 = CARTESIAN_POINT('',(-1.02722794543716,-5.7,2.27921099245176)) ;
#20824 = CARTESIAN_POINT('',(-1.13349364905389,-5.7,2.46326859021798)) ;
#20825 = CARTESIAN_POINT('',(-0.25,-5.7,2.48746859276655)) ;
#20826 = CARTESIAN_POINT('Origin',(0.,-5.7,0.)) ;
#20827 = CARTESIAN_POINT('',(-0.25,-5.7,3.)) ;
#20828 = CARTESIAN_POINT('',(-0.25,-5.7,2.7)) ;
#20829 = CARTESIAN_POINT('',(0.25,-5.7,3.)) ;
#20830 = CARTESIAN_POINT('',(1.83697019872103E-16,-5.7,3.)) ;
#20831 = CARTESIAN_POINT('',(0.25,-5.7,2.48746859276655)) ;
#20832 = CARTESIAN_POINT('',(0.25,-5.7,2.7)) ;
#20833 = CARTESIAN_POINT('',(1.02722794543717,-5.7,2.27921099245176)) ;
#20834 = CARTESIAN_POINT('Origin',(0.,-5.7,0.)) ;
#20835 = CARTESIAN_POINT('',(1.28349364905389,-5.7,2.72307621135332)) ;
#20836 = CARTESIAN_POINT('',(1.13349364905389,-5.7,2.46326859021798)) ;
#20837 = CARTESIAN_POINT('',(1.71650635094611,-5.7,2.47307621135332)) ;
#20838 = CARTESIAN_POINT('',(1.5,-5.7,2.59807621135332)) ;
#20839 = CARTESIAN_POINT('',(1.46024064732938,-5.7,2.02921099245176)) ;
#20840 = CARTESIAN_POINT('',(1.56650635094611,-5.7,2.21326859021798)) ;
#20841 = CARTESIAN_POINT('',(2.02921099245176,-5.7,1.46024064732938)) ;
#20842 = CARTESIAN_POINT('Origin',(0.,-5.7,0.)) ;
#20843 = CARTESIAN_POINT('',(2.47307621135332,-5.7,1.71650635094611)) ;
#20844 = CARTESIAN_POINT('',(2.21326859021798,-5.7,1.56650635094611)) ;
#20845 = CARTESIAN_POINT('',(2.72307621135332,-5.7,1.28349364905389)) ;
#20846 = CARTESIAN_POINT('',(2.59807621135332,-5.7,1.5)) ;
#20847 = CARTESIAN_POINT('',(2.27921099245176,-5.7,1.02722794543716)) ;
#20848 = CARTESIAN_POINT('',(2.46326859021798,-5.7,1.13349364905389)) ;
#20849 = CARTESIAN_POINT('',(2.48746859276655,-5.7,0.25)) ;
#20850 = CARTESIAN_POINT('Origin',(0.,-5.7,0.)) ;
#20851 = CARTESIAN_POINT('',(3.,-5.7,0.25)) ;
#20852 = CARTESIAN_POINT('',(2.7,-5.7,0.25)) ;
#20853 = CARTESIAN_POINT('',(3.,-5.7,-0.25)) ;
#20854 = CARTESIAN_POINT('',(3.,-5.7,0.)) ;
#20855 = CARTESIAN_POINT('',(2.7,-5.7,-0.25)) ;
#20856 = CARTESIAN_POINT('Origin',(1.56650635094611,-6.05,-2.21326859021798)) ;
#20857 = CARTESIAN_POINT('',(1.71650635094611,-6.4,-2.47307621135332)) ;
#20858 = CARTESIAN_POINT('',(1.56650635094611,-6.4,-2.21326859021798)) ;
#20859 = CARTESIAN_POINT('',(1.71650635094611,-6.05,-2.47307621135332)) ;
#20860 = CARTESIAN_POINT('Origin',(1.13349364905389,-6.05,-2.46326859021798)) ;
#20861 = CARTESIAN_POINT('',(1.02722794543717,-6.4,-2.27921099245176)) ;
#20862 = CARTESIAN_POINT('',(1.02722794543717,-6.05,-2.27921099245176)) ;
#20863 = CARTESIAN_POINT('',(1.28349364905389,-6.4,-2.72307621135332)) ;
#20864 = CARTESIAN_POINT('',(1.28349364905389,-6.05,-2.72307621135332)) ;
#20865 = CARTESIAN_POINT('',(1.13349364905389,-6.4,-2.46326859021798)) ;
#20866 = CARTESIAN_POINT('Origin',(1.5,-6.05,-2.59807621135332)) ;
#20867 = CARTESIAN_POINT('',(1.5,-6.4,-2.59807621135332)) ;
#20868 = CARTESIAN_POINT('Origin',(0.,-6.05,0.)) ;
#20869 = CARTESIAN_POINT('',(0.25,-6.4,-2.48746859276655)) ;
#20870 = CARTESIAN_POINT('Origin',(0.,-6.4,0.)) ;
#20871 = CARTESIAN_POINT('',(0.25,-6.05,-2.48746859276655)) ;
#20872 = CARTESIAN_POINT('Origin',(-0.25,-6.05,-2.7)) ;
#20873 = CARTESIAN_POINT('',(-0.25,-6.4,-2.48746859276655)) ;
#20874 = CARTESIAN_POINT('',(-0.25,-6.05,-2.48746859276655)) ;
#20875 = CARTESIAN_POINT('',(-0.250000000000001,-6.4,-3.)) ;
#20876 = CARTESIAN_POINT('',(-0.250000000000001,-6.05,-3.)) ;
#20877 = CARTESIAN_POINT('',(-0.25,-6.4,-2.7)) ;
#20878 = CARTESIAN_POINT('Origin',(0.25,-6.05,-2.7)) ;
#20879 = CARTESIAN_POINT('',(0.249999999999999,-6.4,-3.)) ;
#20880 = CARTESIAN_POINT('',(0.25,-6.4,-2.7)) ;
#20881 = CARTESIAN_POINT('',(0.249999999999999,-6.05,-3.)) ;
#20882 = CARTESIAN_POINT('Origin',(-5.51091059616309E-16,-6.05,-3.)) ;
#20883 = CARTESIAN_POINT('',(-5.51091059616309E-16,-6.4,-3.)) ;
#20884 = CARTESIAN_POINT('Origin',(0.,-6.05,0.)) ;
#20885 = CARTESIAN_POINT('',(-1.02722794543717,-6.4,-2.27921099245176)) ;
#20886 = CARTESIAN_POINT('Origin',(0.,-6.4,0.)) ;
#20887 = CARTESIAN_POINT('',(-1.02722794543717,-6.05,-2.27921099245176)) ;
#20888 = CARTESIAN_POINT('Origin',(-1.13349364905389,-6.05,-2.46326859021798)) ;
#20889 = CARTESIAN_POINT('',(-1.28349364905389,-6.4,-2.72307621135332)) ;
#20890 = CARTESIAN_POINT('',(-1.13349364905389,-6.4,-2.46326859021798)) ;
#20891 = CARTESIAN_POINT('',(-1.28349364905389,-6.05,-2.72307621135332)) ;
#20892 = CARTESIAN_POINT('Origin',(-1.56650635094611,-6.05,-2.21326859021798)) ;
#20893 = CARTESIAN_POINT('',(-1.46024064732939,-6.4,-2.02921099245176)) ;
#20894 = CARTESIAN_POINT('',(-1.46024064732939,-6.05,-2.02921099245176)) ;
#20895 = CARTESIAN_POINT('',(-1.71650635094611,-6.4,-2.47307621135332)) ;
#20896 = CARTESIAN_POINT('',(-1.71650635094611,-6.05,-2.47307621135332)) ;
#20897 = CARTESIAN_POINT('',(-1.56650635094611,-6.4,-2.21326859021798)) ;
#20898 = CARTESIAN_POINT('Origin',(-1.5,-6.05,-2.59807621135332)) ;
#20899 = CARTESIAN_POINT('',(-1.5,-6.4,-2.59807621135332)) ;
#20900 = CARTESIAN_POINT('Origin',(0.,-6.05,0.)) ;
#20901 = CARTESIAN_POINT('',(-2.02921099245176,-6.4,-1.46024064732938)) ;
#20902 = CARTESIAN_POINT('Origin',(0.,-6.4,0.)) ;
#20903 = CARTESIAN_POINT('',(-2.02921099245176,-6.05,-1.46024064732938)) ;
#20904 = CARTESIAN_POINT('Origin',(-2.46326859021798,-6.05,-1.13349364905389)) ;
#20905 = CARTESIAN_POINT('',(-2.27921099245176,-6.4,-1.02722794543717)) ;
#20906 = CARTESIAN_POINT('',(-2.27921099245176,-6.05,-1.02722794543717)) ;
#20907 = CARTESIAN_POINT('',(-2.72307621135332,-6.4,-1.28349364905389)) ;
#20908 = CARTESIAN_POINT('',(-2.72307621135332,-6.05,-1.28349364905389)) ;
#20909 = CARTESIAN_POINT('',(-2.46326859021798,-6.4,-1.13349364905389)) ;
#20910 = CARTESIAN_POINT('Origin',(-2.21326859021798,-6.05,-1.56650635094611)) ;
#20911 = CARTESIAN_POINT('',(-2.47307621135332,-6.4,-1.71650635094611)) ;
#20912 = CARTESIAN_POINT('',(-2.21326859021798,-6.4,-1.56650635094611)) ;
#20913 = CARTESIAN_POINT('',(-2.47307621135332,-6.05,-1.71650635094611)) ;
#20914 = CARTESIAN_POINT('Origin',(-2.59807621135332,-6.05,-1.5)) ;
#20915 = CARTESIAN_POINT('',(-2.59807621135332,-6.4,-1.5)) ;
#20916 = CARTESIAN_POINT('Origin',(0.,-6.05,0.)) ;
#20917 = CARTESIAN_POINT('',(-2.48746859276655,-6.4,-0.25)) ;
#20918 = CARTESIAN_POINT('Origin',(0.,-6.4,0.)) ;
#20919 = CARTESIAN_POINT('',(-2.48746859276655,-6.05,-0.25)) ;
#20920 = CARTESIAN_POINT('Origin',(-2.7,-6.05,-0.25)) ;
#20921 = CARTESIAN_POINT('',(-3.,-6.4,-0.25)) ;
#20922 = CARTESIAN_POINT('',(-2.7,-6.4,-0.25)) ;
#20923 = CARTESIAN_POINT('',(-3.,-6.05,-0.25)) ;
#20924 = CARTESIAN_POINT('Origin',(-2.7,-6.05,0.25)) ;
#20925 = CARTESIAN_POINT('',(-2.48746859276655,-6.4,0.25)) ;
#20926 = CARTESIAN_POINT('',(-2.48746859276655,-6.05,0.25)) ;
#20927 = CARTESIAN_POINT('',(-3.,-6.4,0.25)) ;
#20928 = CARTESIAN_POINT('',(-3.,-6.05,0.25)) ;
#20929 = CARTESIAN_POINT('',(-2.7,-6.4,0.25)) ;
#20930 = CARTESIAN_POINT('Origin',(-3.,-6.05,3.67394039744206E-16)) ;
#20931 = CARTESIAN_POINT('',(-3.,-6.4,3.67394039744206E-16)) ;
#20932 = CARTESIAN_POINT('Origin',(0.,-6.05,0.)) ;
#20933 = CARTESIAN_POINT('',(-2.27921099245176,-6.4,1.02722794543717)) ;
#20934 = CARTESIAN_POINT('Origin',(0.,-6.4,0.)) ;
#20935 = CARTESIAN_POINT('',(-2.27921099245176,-6.05,1.02722794543716)) ;
#20936 = CARTESIAN_POINT('Origin',(-2.21326859021798,-6.05,1.56650635094611)) ;
#20937 = CARTESIAN_POINT('',(-2.02921099245176,-6.4,1.46024064732938)) ;
#20938 = CARTESIAN_POINT('',(-2.02921099245176,-6.05,1.46024064732938)) ;
#20939 = CARTESIAN_POINT('',(-2.47307621135332,-6.4,1.71650635094611)) ;
#20940 = CARTESIAN_POINT('',(-2.47307621135332,-6.05,1.71650635094611)) ;
#20941 = CARTESIAN_POINT('',(-2.21326859021798,-6.4,1.56650635094611)) ;
#20942 = CARTESIAN_POINT('Origin',(-2.46326859021798,-6.05,1.13349364905389)) ;
#20943 = CARTESIAN_POINT('',(-2.72307621135332,-6.4,1.28349364905389)) ;
#20944 = CARTESIAN_POINT('',(-2.46326859021798,-6.4,1.13349364905389)) ;
#20945 = CARTESIAN_POINT('',(-2.72307621135332,-6.05,1.28349364905389)) ;
#20946 = CARTESIAN_POINT('Origin',(-2.59807621135332,-6.05,1.5)) ;
#20947 = CARTESIAN_POINT('',(-2.59807621135332,-6.4,1.5)) ;
#20948 = CARTESIAN_POINT('Origin',(0.,-6.05,0.)) ;
#20949 = CARTESIAN_POINT('',(-1.46024064732938,-6.4,2.02921099245176)) ;
#20950 = CARTESIAN_POINT('Origin',(0.,-6.4,0.)) ;
#20951 = CARTESIAN_POINT('',(-1.46024064732938,-6.05,2.02921099245176)) ;
#20952 = CARTESIAN_POINT('Origin',(-1.56650635094611,-6.05,2.21326859021798)) ;
#20953 = CARTESIAN_POINT('',(-1.71650635094611,-6.4,2.47307621135332)) ;
#20954 = CARTESIAN_POINT('',(-1.56650635094611,-6.4,2.21326859021798)) ;
#20955 = CARTESIAN_POINT('',(-1.71650635094611,-6.05,2.47307621135332)) ;
#20956 = CARTESIAN_POINT('Origin',(-1.13349364905389,-6.05,2.46326859021798)) ;
#20957 = CARTESIAN_POINT('',(-1.02722794543716,-6.4,2.27921099245176)) ;
#20958 = CARTESIAN_POINT('',(-1.02722794543716,-6.05,2.27921099245176)) ;
#20959 = CARTESIAN_POINT('',(-1.28349364905389,-6.4,2.72307621135332)) ;
#20960 = CARTESIAN_POINT('',(-1.28349364905389,-6.05,2.72307621135332)) ;
#20961 = CARTESIAN_POINT('',(-1.13349364905389,-6.4,2.46326859021798)) ;
#20962 = CARTESIAN_POINT('Origin',(-1.5,-6.05,2.59807621135332)) ;
#20963 = CARTESIAN_POINT('',(-1.5,-6.4,2.59807621135332)) ;
#20964 = CARTESIAN_POINT('Origin',(0.,-6.05,0.)) ;
#20965 = CARTESIAN_POINT('',(-0.25,-6.4,2.48746859276655)) ;
#20966 = CARTESIAN_POINT('Origin',(0.,-6.4,0.)) ;
#20967 = CARTESIAN_POINT('',(-0.25,-6.05,2.48746859276655)) ;
#20968 = CARTESIAN_POINT('Origin',(0.25,-6.05,2.7)) ;
#20969 = CARTESIAN_POINT('',(0.25,-6.4,2.48746859276655)) ;
#20970 = CARTESIAN_POINT('',(0.25,-6.05,2.48746859276655)) ;
#20971 = CARTESIAN_POINT('',(0.25,-6.4,3.)) ;
#20972 = CARTESIAN_POINT('',(0.25,-6.05,3.)) ;
#20973 = CARTESIAN_POINT('',(0.25,-6.4,2.7)) ;
#20974 = CARTESIAN_POINT('Origin',(-0.25,-6.05,2.7)) ;
#20975 = CARTESIAN_POINT('',(-0.25,-6.4,3.)) ;
#20976 = CARTESIAN_POINT('',(-0.25,-6.4,2.7)) ;
#20977 = CARTESIAN_POINT('',(-0.25,-6.05,3.)) ;
#20978 = CARTESIAN_POINT('Origin',(1.83697019872103E-16,-6.05,3.)) ;
#20979 = CARTESIAN_POINT('',(1.83697019872103E-16,-6.4,3.)) ;
#20980 = CARTESIAN_POINT('Origin',(0.,-6.05,0.)) ;
#20981 = CARTESIAN_POINT('',(1.02722794543717,-6.4,2.27921099245176)) ;
#20982 = CARTESIAN_POINT('Origin',(0.,-6.4,0.)) ;
#20983 = CARTESIAN_POINT('',(1.02722794543717,-6.05,2.27921099245176)) ;
#20984 = CARTESIAN_POINT('Origin',(1.13349364905389,-6.05,2.46326859021798)) ;
#20985 = CARTESIAN_POINT('',(1.28349364905389,-6.4,2.72307621135332)) ;
#20986 = CARTESIAN_POINT('',(1.13349364905389,-6.4,2.46326859021798)) ;
#20987 = CARTESIAN_POINT('',(1.28349364905389,-6.05,2.72307621135332)) ;
#20988 = CARTESIAN_POINT('Origin',(1.56650635094611,-6.05,2.21326859021798)) ;
#20989 = CARTESIAN_POINT('',(1.46024064732938,-6.4,2.02921099245176)) ;
#20990 = CARTESIAN_POINT('',(1.46024064732938,-6.05,2.02921099245176)) ;
#20991 = CARTESIAN_POINT('',(1.71650635094611,-6.4,2.47307621135332)) ;
#20992 = CARTESIAN_POINT('',(1.71650635094611,-6.05,2.47307621135332)) ;
#20993 = CARTESIAN_POINT('',(1.56650635094611,-6.4,2.21326859021798)) ;
#20994 = CARTESIAN_POINT('Origin',(1.5,-6.05,2.59807621135332)) ;
#20995 = CARTESIAN_POINT('',(1.5,-6.4,2.59807621135332)) ;
#20996 = CARTESIAN_POINT('Origin',(0.,-6.05,0.)) ;
#20997 = CARTESIAN_POINT('',(2.02921099245176,-6.4,1.46024064732938)) ;
#20998 = CARTESIAN_POINT('Origin',(0.,-6.4,0.)) ;
#20999 = CARTESIAN_POINT('',(2.02921099245176,-6.05,1.46024064732938)) ;
#21000 = CARTESIAN_POINT('Origin',(2.46326859021798,-6.05,1.13349364905389)) ;
#21001 = CARTESIAN_POINT('',(2.27921099245176,-6.4,1.02722794543717)) ;
#21002 = CARTESIAN_POINT('',(2.27921099245176,-6.05,1.02722794543716)) ;
#21003 = CARTESIAN_POINT('',(2.72307621135332,-6.4,1.28349364905389)) ;
#21004 = CARTESIAN_POINT('',(2.72307621135332,-6.05,1.28349364905389)) ;
#21005 = CARTESIAN_POINT('',(2.46326859021798,-6.4,1.13349364905389)) ;
#21006 = CARTESIAN_POINT('Origin',(2.21326859021798,-6.05,1.56650635094611)) ;
#21007 = CARTESIAN_POINT('',(2.47307621135332,-6.4,1.71650635094611)) ;
#21008 = CARTESIAN_POINT('',(2.21326859021798,-6.4,1.56650635094611)) ;
#21009 = CARTESIAN_POINT('',(2.47307621135332,-6.05,1.71650635094611)) ;
#21010 = CARTESIAN_POINT('Origin',(2.59807621135332,-6.05,1.5)) ;
#21011 = CARTESIAN_POINT('',(2.59807621135332,-6.4,1.5)) ;
#21012 = CARTESIAN_POINT('Origin',(0.,-6.05,0.)) ;
#21013 = CARTESIAN_POINT('',(2.48746859276655,-6.4,0.25)) ;
#21014 = CARTESIAN_POINT('Origin',(0.,-6.4,0.)) ;
#21015 = CARTESIAN_POINT('',(2.48746859276655,-6.05,0.25)) ;
#21016 = CARTESIAN_POINT('Origin',(2.7,-6.05,0.25)) ;
#21017 = CARTESIAN_POINT('',(3.,-6.4,0.25)) ;
#21018 = CARTESIAN_POINT('',(2.7,-6.4,0.25)) ;
#21019 = CARTESIAN_POINT('',(3.,-6.05,0.25)) ;
#21020 = CARTESIAN_POINT('Origin',(2.7,-6.05,-0.25)) ;
#21021 = CARTESIAN_POINT('',(3.,-6.4,-0.25)) ;
#21022 = CARTESIAN_POINT('',(3.,-6.05,-0.25)) ;
#21023 = CARTESIAN_POINT('',(2.7,-6.4,-0.25)) ;
#21024 = CARTESIAN_POINT('Origin',(3.,-6.05,0.)) ;
#21025 = CARTESIAN_POINT('',(3.,-6.4,0.)) ;
#21026 = CARTESIAN_POINT('Origin',(0.,-6.25,0.)) ;
#21027 = CARTESIAN_POINT('',(-1.4,-6.4,1.71450551880629E-16)) ;
#21028 = CARTESIAN_POINT('Origin',(0.,-6.4,0.)) ;
#21029 = CARTESIAN_POINT('',(-1.4,-6.25,1.71450551880629E-16)) ;
#21030 = CARTESIAN_POINT('Origin',(0.,-6.4,0.)) ;
#21031 = CARTESIAN_POINT('',(0.,0.,0.)) ;
#21032 = CARTESIAN_POINT('Origin',(0.75,-6.15,0.25)) ;
#21033 = CARTESIAN_POINT('',(1.,-6.6,0.25)) ;
#21034 = CARTESIAN_POINT('',(1.,-5.7,0.25)) ;
#21035 = CARTESIAN_POINT('',(1.,-6.15,0.25)) ;
#21036 = CARTESIAN_POINT('',(0.5,-5.7,0.25)) ;
#21037 = CARTESIAN_POINT('',(0.75,-5.7,0.25)) ;
#21038 = CARTESIAN_POINT('',(0.5,-6.6,0.25)) ;
#21039 = CARTESIAN_POINT('',(0.5,-6.15,0.25)) ;
#21040 = CARTESIAN_POINT('',(0.75,-6.6,0.25)) ;
#21041 = CARTESIAN_POINT('Origin',(0.75,-6.15,-0.25)) ;
#21042 = CARTESIAN_POINT('',(1.,-5.7,-0.25)) ;
#21043 = CARTESIAN_POINT('',(1.,-6.6,-0.25)) ;
#21044 = CARTESIAN_POINT('',(1.,-6.15,-0.25)) ;
#21045 = CARTESIAN_POINT('',(0.5,-6.6,-0.25)) ;
#21046 = CARTESIAN_POINT('',(0.75,-6.6,-0.25)) ;
#21047 = CARTESIAN_POINT('',(0.5,-5.7,-0.25)) ;
#21048 = CARTESIAN_POINT('',(0.5,-6.15,-0.25)) ;
#21049 = CARTESIAN_POINT('',(0.75,-5.7,-0.25)) ;
#21050 = CARTESIAN_POINT('Origin',(0.75,-6.6,0.)) ;
#21051 = CARTESIAN_POINT('',(0.5,-6.6,0.)) ;
#21052 = CARTESIAN_POINT('',(1.,-6.6,0.)) ;
#21053 = CARTESIAN_POINT('Origin',(0.5,-6.15,0.)) ;
#21054 = CARTESIAN_POINT('',(0.5,-5.7,0.)) ;
#21055 = CARTESIAN_POINT('Origin',(0.75,-5.7,0.)) ;
#21056 = CARTESIAN_POINT('',(1.,-5.7,0.)) ;
#21057 = CARTESIAN_POINT('Origin',(1.,-6.15,0.)) ;
#21058 = CARTESIAN_POINT('',(0.,0.,0.)) ;
#21059 = CARTESIAN_POINT('Origin',(0.,-0.7,0.)) ;
#21060 = CARTESIAN_POINT('',(-10.2,-1.4,1.2491397351303E-15)) ;
#21061 = CARTESIAN_POINT('Origin',(0.,-1.4,0.)) ;
#21062 = CARTESIAN_POINT('',(-10.2,0.,-1.2491397351303E-15)) ;
#21063 = CARTESIAN_POINT('',(-10.2,-0.7,1.2491397351303E-15)) ;
#21064 = CARTESIAN_POINT('Origin',(0.,0.,0.)) ;
#21065 = CARTESIAN_POINT('Origin',(0.,-0.7,0.)) ;
#21066 = CARTESIAN_POINT('',(-11.1,0.,1.35935794705356E-15)) ;
#21067 = CARTESIAN_POINT('Origin',(0.,0.,0.)) ;
#21068 = CARTESIAN_POINT('',(-11.1,-1.4,1.35935794705356E-15)) ;
#21069 = CARTESIAN_POINT('',(-11.1,-0.7,1.35935794705356E-15)) ;
#21070 = CARTESIAN_POINT('Origin',(0.,-1.4,0.)) ;
#21071 = CARTESIAN_POINT('Origin',(0.,-1.4,0.)) ;
#21072 = CARTESIAN_POINT('Origin',(0.,0.,0.)) ;
#21073 = CARTESIAN_POINT('',(0.,0.,0.)) ;
#21074 = CARTESIAN_POINT('Origin',(0.,1.05,0.2)) ;
#21075 = CARTESIAN_POINT('',(-0.8,1.8,0.2)) ;
#21076 = CARTESIAN_POINT('',(0.8,1.8,0.2)) ;
#21077 = CARTESIAN_POINT('',(0.,1.8,0.2)) ;
#21078 = CARTESIAN_POINT('',(-0.8,0.2,0.2)) ;
#21079 = CARTESIAN_POINT('',(-0.8,1.05,0.2)) ;
#21080 = CARTESIAN_POINT('',(0.8,0.2,0.2)) ;
#21081 = CARTESIAN_POINT('',(0.,0.2,0.2)) ;
#21082 = CARTESIAN_POINT('',(0.8,1.05,0.2)) ;
#21083 = CARTESIAN_POINT('Origin',(0.8,1.05,0.7)) ;
#21084 = CARTESIAN_POINT('',(0.8,1.8,1.1)) ;
#21085 = CARTESIAN_POINT('',(0.8,1.8,0.625)) ;
#21086 = CARTESIAN_POINT('',(0.8,0.2,1.1)) ;
#21087 = CARTESIAN_POINT('',(0.8,0.2,0.7)) ;
#21088 = CARTESIAN_POINT('',(0.8,0.975,1.1)) ;
#21089 = CARTESIAN_POINT('Origin',(0.,0.2,0.7)) ;
#21090 = CARTESIAN_POINT('',(-0.8,0.2,1.1)) ;
#21091 = CARTESIAN_POINT('',(0.,0.2,1.1)) ;
#21092 = CARTESIAN_POINT('',(-0.8,0.2,0.7)) ;
#21093 = CARTESIAN_POINT('Origin',(-0.8,1.05,0.7)) ;
#21094 = CARTESIAN_POINT('',(-0.8,1.8,1.1)) ;
#21095 = CARTESIAN_POINT('',(-0.8,1.8,0.625)) ;
#21096 = CARTESIAN_POINT('',(-0.8,0.975,1.1)) ;
#21097 = CARTESIAN_POINT('Origin',(0.,1.8,0.55)) ;
#21098 = CARTESIAN_POINT('',(1.,1.8,1.1)) ;
#21099 = CARTESIAN_POINT('',(0.,1.8,1.1)) ;
#21100 = CARTESIAN_POINT('',(1.,1.8,0.)) ;
#21101 = CARTESIAN_POINT('',(1.,1.8,0.55)) ;
#21102 = CARTESIAN_POINT('',(-1.,1.8,0.)) ;
#21103 = CARTESIAN_POINT('',(0.,1.8,0.)) ;
#21104 = CARTESIAN_POINT('',(-1.,1.8,1.1)) ;
#21105 = CARTESIAN_POINT('',(-1.,1.8,0.55)) ;
#21106 = CARTESIAN_POINT('',(0.,1.8,1.1)) ;
#21107 = CARTESIAN_POINT('Origin',(0.,0.9,1.1)) ;
#21108 = CARTESIAN_POINT('',(-1.,0.,1.1)) ;
#21109 = CARTESIAN_POINT('',(-1.,0.9,1.1)) ;
#21110 = CARTESIAN_POINT('',(1.,0.,1.1)) ;
#21111 = CARTESIAN_POINT('',(0.,0.,1.1)) ;
#21112 = CARTESIAN_POINT('',(1.,0.9,1.1)) ;
#21113 = CARTESIAN_POINT('Origin',(0.,0.9,0.)) ;
#21114 = CARTESIAN_POINT('',(1.,0.,0.)) ;
#21115 = CARTESIAN_POINT('',(1.,0.9,0.)) ;
#21116 = CARTESIAN_POINT('',(-1.,0.,0.)) ;
#21117 = CARTESIAN_POINT('',(0.,0.,0.)) ;
#21118 = CARTESIAN_POINT('',(-1.,0.9,0.)) ;
#21119 = CARTESIAN_POINT('Origin',(0.,0.,0.55)) ;
#21120 = CARTESIAN_POINT('',(-1.,0.,0.55)) ;
#21121 = CARTESIAN_POINT('',(1.,0.,0.55)) ;
#21122 = CARTESIAN_POINT('Origin',(-1.,0.9,0.55)) ;
#21123 = CARTESIAN_POINT('Origin',(1.,0.9,0.55)) ;
#21124 = CARTESIAN_POINT('',(0.,0.,0.)) ;
#21125 = CARTESIAN_POINT('Origin',(-6.43477332219942,-0.07,5.39941592136693)) ;
#21126 = CARTESIAN_POINT('',(-6.68477332219942,0.1,5.39941592136693)) ;
#21127 = CARTESIAN_POINT('Origin',(-6.43477332219942,0.1,5.39941592136693)) ;
#21128 = CARTESIAN_POINT('',(-6.68477332219942,-0.24,5.39941592136693)) ;
#21129 = CARTESIAN_POINT('',(-6.68477332219942,-0.07,5.39941592136693)) ;
#21130 = CARTESIAN_POINT('Origin',(-6.43477332219942,-0.24,5.39941592136693)) ;
#21131 = CARTESIAN_POINT('Origin',(-6.43477332219942,-0.24,5.39941592136693)) ;
#21132 = CARTESIAN_POINT('Origin',(-6.1946255125913,0.2,8.84684207832111)) ;
#21133 = CARTESIAN_POINT('',(-6.4046255125913,0.1,8.84684207832111)) ;
#21134 = CARTESIAN_POINT('Origin',(-6.1946255125913,0.1,8.84684207832111)) ;
#21135 = CARTESIAN_POINT('',(-6.4046255125913,0.3,8.84684207832111)) ;
#21136 = CARTESIAN_POINT('',(-6.4046255125913,0.2,8.84684207832111)) ;
#21137 = CARTESIAN_POINT('Origin',(-6.1946255125913,0.3,8.84684207832111)) ;
#21138 = CARTESIAN_POINT('Origin',(-6.1946255125913,0.2,8.84684207832111)) ;
#21139 = CARTESIAN_POINT('',(-6.61450601525,0.1,8.57536396965105)) ;
#21140 = CARTESIAN_POINT('',(-6.61450601525,0.3,8.57536396965105)) ;
#21141 = CARTESIAN_POINT('',(-6.61450601525,0.2,8.57536396965105)) ;
#21142 = CARTESIAN_POINT('',(-6.57281103765899,0.1,9.17391349044585)) ;
#21143 = CARTESIAN_POINT('Origin',(-6.1946255125913,0.1,8.84684207832111)) ;
#21144 = CARTESIAN_POINT('',(-6.57281103765899,0.3,9.17391349044585)) ;
#21145 = CARTESIAN_POINT('',(-6.57281103765899,0.2,9.17391349044585)) ;
#21146 = CARTESIAN_POINT('Origin',(-6.1946255125913,0.3,8.84684207832111)) ;
#21147 = CARTESIAN_POINT('Origin',(-6.1946255125913,0.2,8.84684207832111)) ;
#21148 = CARTESIAN_POINT('',(-5.86755410046656,0.3,9.22502760338881)) ;
#21149 = CARTESIAN_POINT('',(-5.86755410046656,0.1,9.22502760338881)) ;
#21150 = CARTESIAN_POINT('',(-5.86755410046656,0.2,9.22502760338881)) ;
#21151 = CARTESIAN_POINT('',(-6.46610362126136,0.3,9.26672258097981)) ;
#21152 = CARTESIAN_POINT('Origin',(-6.1946255125913,0.3,8.84684207832111)) ;
#21153 = CARTESIAN_POINT('',(-6.46610362126136,0.1,9.26672258097981)) ;
#21154 = CARTESIAN_POINT('',(-6.46610362126136,0.2,9.26672258097981)) ;
#21155 = CARTESIAN_POINT('Origin',(-6.1946255125913,0.1,8.84684207832111)) ;
#21156 = CARTESIAN_POINT('Origin',(-6.1946255125913,0.2,8.84684207832111)) ;
#21157 = CARTESIAN_POINT('',(-5.77474500993259,0.1,9.11832018699117)) ;
#21158 = CARTESIAN_POINT('',(-5.77474500993259,0.3,9.11832018699117)) ;
#21159 = CARTESIAN_POINT('',(-5.77474500993259,0.2,9.11832018699117)) ;
#21160 = CARTESIAN_POINT('',(-5.8164399875236,0.1,8.51977066619637)) ;
#21161 = CARTESIAN_POINT('Origin',(-6.1946255125913,0.1,8.84684207832111)) ;
#21162 = CARTESIAN_POINT('',(-5.8164399875236,0.3,8.51977066619637)) ;
#21163 = CARTESIAN_POINT('',(-5.8164399875236,0.2,8.51977066619637)) ;
#21164 = CARTESIAN_POINT('Origin',(-6.1946255125913,0.3,8.84684207832111)) ;
#21165 = CARTESIAN_POINT('Origin',(-5.91566640353216,0.2,7.09533234811668)) ;
#21166 = CARTESIAN_POINT('',(-6.06353696006355,0.1,4.97258625577639)) ;
#21167 = CARTESIAN_POINT('',(-5.91566640353216,0.1,7.09533234811668)) ;
#21168 = CARTESIAN_POINT('',(-6.06353696006355,0.3,4.97258625577639)) ;
#21169 = CARTESIAN_POINT('',(-6.06353696006355,0.2,4.97258625577639)) ;
#21170 = CARTESIAN_POINT('',(-5.91566640353216,0.3,7.09533234811668)) ;
#21171 = CARTESIAN_POINT('Origin',(-5.91566640353216,0.2,7.09533234811668)) ;
#21172 = CARTESIAN_POINT('',(-5.76779584700076,0.3,9.21807844045697)) ;
#21173 = CARTESIAN_POINT('',(-5.91566640353216,0.3,7.09533234811668)) ;
#21174 = CARTESIAN_POINT('',(-5.76779584700076,0.1,9.21807844045697)) ;
#21175 = CARTESIAN_POINT('',(-5.76779584700076,0.2,9.21807844045697)) ;
#21176 = CARTESIAN_POINT('',(-5.91566640353216,0.1,7.09533234811668)) ;
#21177 = CARTESIAN_POINT('Origin',(-6.16682886086396,0.2,9.24587509218431)) ;
#21178 = CARTESIAN_POINT('',(-6.56586187472716,0.3,9.27367174391165)) ;
#21179 = CARTESIAN_POINT('',(-6.16682886086396,0.3,9.24587509218431)) ;
#21180 = CARTESIAN_POINT('',(-6.56586187472716,0.1,9.27367174391165)) ;
#21181 = CARTESIAN_POINT('',(-6.56586187472716,0.2,9.27367174391165)) ;
#21182 = CARTESIAN_POINT('',(-6.16682886086396,0.1,9.24587509218431)) ;
#21183 = CARTESIAN_POINT('Origin',(-6.31469941739536,0.3,7.12312899984402)) ;
#21184 = CARTESIAN_POINT('',(-6.16682886086396,0.3,9.24587509218431)) ;
#21185 = CARTESIAN_POINT('',(-6.86160298778995,0.3,5.02817955923107)) ;
#21186 = CARTESIAN_POINT('',(-6.46256997392675,0.3,5.00038290750373)) ;
#21187 = CARTESIAN_POINT('',(-6.71373243125856,0.3,7.15092565157136)) ;
#21188 = CARTESIAN_POINT('',(-6.71373243125856,0.3,7.15092565157136)) ;
#21189 = CARTESIAN_POINT('Origin',(-6.71373243125856,0.2,7.15092565157136)) ;
#21190 = CARTESIAN_POINT('',(-6.71373243125856,0.1,7.15092565157136)) ;
#21191 = CARTESIAN_POINT('Origin',(-6.71373243125856,0.2,7.15092565157136)) ;
#21192 = CARTESIAN_POINT('',(-6.86160298778995,0.1,5.02817955923107)) ;
#21193 = CARTESIAN_POINT('',(-6.86160298778995,0.2,5.02817955923107)) ;
#21194 = CARTESIAN_POINT('',(-6.71373243125856,0.1,7.15092565157136)) ;
#21195 = CARTESIAN_POINT('Origin',(-6.31469941739536,0.1,7.12312899984402)) ;
#21196 = CARTESIAN_POINT('',(-6.16682886086396,0.1,9.24587509218431)) ;
#21197 = CARTESIAN_POINT('',(-6.46256997392675,0.1,5.00038290750373)) ;
#21198 = CARTESIAN_POINT('Origin',(-6.16682886086396,0.2,9.24587509218431)) ;
#21199 = CARTESIAN_POINT('Origin',(-6.46256997392675,0.2,5.00038290750373)) ;
#21200 = CARTESIAN_POINT('',(0.,0.,0.)) ;
#21201 = CARTESIAN_POINT('Origin',(-6.1946255125913,1.975,8.84684207832111)) ;
#21202 = CARTESIAN_POINT('',(-6.3946255125913,3.9,8.84684207832111)) ;
#21203 = CARTESIAN_POINT('Origin',(-6.1946255125913,3.9,8.84684207832111)) ;
#21204 = CARTESIAN_POINT('',(-6.3946255125913,0.05,8.84684207832111)) ;
#21205 = CARTESIAN_POINT('',(-6.3946255125913,1.975,8.84684207832111)) ;
#21206 = CARTESIAN_POINT('Origin',(-6.1946255125913,0.0499999999999998,8.84684207832111)) ;
#21207 = CARTESIAN_POINT('Origin',(-6.1946255125913,0.0499999999999998,8.84684207832111)) ;
#21208 = CARTESIAN_POINT('Origin',(-6.1946255125913,3.9,8.84684207832111)) ;
#21209 = CARTESIAN_POINT('',(0.,0.,0.)) ;
#21210 = CARTESIAN_POINT('Origin',(-5.94713813917601,0.815,9.0943294517364)) ;
#21211 = CARTESIAN_POINT('',(-5.9449992070826,0.765091584487187,9.092190519643)) ;
#21212 = CARTESIAN_POINT('',(-5.94927707126941,0.864908415512813,9.09646838382981)) ;
#21213 = CARTESIAN_POINT('Origin',(-5.94713813917601,0.815,9.0943294517364)) ;
#21214 = CARTESIAN_POINT('Origin',(-5.94713813917601,0.815,9.0943294517364)) ;
#21215 = CARTESIAN_POINT('Origin',(-6.1946255125913,0.8,9.19684207832111)) ;
#21216 = CARTESIAN_POINT('',(-6.19160060581581,0.750091584487187,9.19684207832111)) ;
#21217 = CARTESIAN_POINT('',(-6.19765041936679,0.849908415512813,9.19684207832111)) ;
#21218 = CARTESIAN_POINT('Origin',(-6.1946255125913,0.8,9.19684207832111)) ;
#21219 = CARTESIAN_POINT('',(-6.21393318998988,0.806677582745637,9.24247784808724)) ;
#21220 = CARTESIAN_POINT('Origin',(-6.1946255125913,0.8,9.19684207832111)) ;
#21221 = CARTESIAN_POINT('',(-6.21375968420955,0.8,9.24303605494667)) ;
#21222 = CARTESIAN_POINT('Origin',(-6.1946255125913,0.8,9.19684207832111)) ;
#21223 = CARTESIAN_POINT('',(-6.1946255125913,0.8,9.24684207832111)) ;
#21224 = CARTESIAN_POINT('Origin',(-6.1946255125913,0.8,9.19684207832111)) ;
#21225 = CARTESIAN_POINT('Origin',(-6.1946255125913,0.8,9.19684207832111)) ;
#21226 = CARTESIAN_POINT('Origin',(-6.44211288600659,0.785,9.0943294517364)) ;
#21227 = CARTESIAN_POINT('',(-6.43997395391319,0.735091584487187,9.09646838382981)) ;
#21228 = CARTESIAN_POINT('',(-6.46142056340518,0.791677582745637,9.13996522150253)) ;
#21229 = CARTESIAN_POINT('Origin',(-6.44211288600659,0.785,9.0943294517364)) ;
#21230 = CARTESIAN_POINT('',(-6.4442518181,0.834908415512813,9.092190519643)) ;
#21231 = CARTESIAN_POINT('Origin',(-6.44211288600659,0.785,9.0943294517364)) ;
#21232 = CARTESIAN_POINT('',(-6.48831924755442,0.786155771164016,9.11339870304649)) ;
#21233 = CARTESIAN_POINT('Origin',(-6.44211288600659,0.785,9.0943294517364)) ;
#21234 = CARTESIAN_POINT('Origin',(-6.44211288600659,0.785,9.0943294517364)) ;
#21235 = CARTESIAN_POINT('Origin',(-6.5446255125913,0.77,8.84684207832111)) ;
#21236 = CARTESIAN_POINT('',(-6.5446255125913,0.720091584487187,8.8498669850966)) ;
#21237 = CARTESIAN_POINT('',(-6.59083187413913,0.771155771164016,8.8659113296312)) ;
#21238 = CARTESIAN_POINT('Origin',(-6.5446255125913,0.77,8.84684207832111)) ;
#21239 = CARTESIAN_POINT('',(-6.5446255125913,0.819908415512813,8.84381717154562)) ;
#21240 = CARTESIAN_POINT('Origin',(-6.5446255125913,0.77,8.84684207832111)) ;
#21241 = CARTESIAN_POINT('',(-6.59083187413913,0.768844228835984,8.82777282701102)) ;
#21242 = CARTESIAN_POINT('Origin',(-6.5446255125913,0.77,8.84684207832111)) ;
#21243 = CARTESIAN_POINT('Origin',(-6.5446255125913,0.77,8.84684207832111)) ;
#21244 = CARTESIAN_POINT('Origin',(-6.44211288600659,0.755,8.59935470490582)) ;
#21245 = CARTESIAN_POINT('',(-6.4442518181,0.705091584487187,8.60149363699922)) ;
#21246 = CARTESIAN_POINT('',(-6.48831924755442,0.753844228835984,8.58028545359573)) ;
#21247 = CARTESIAN_POINT('Origin',(-6.44211288600659,0.755,8.59935470490582)) ;
#21248 = CARTESIAN_POINT('',(-6.43997395391318,0.804908415512813,8.59721577281241)) ;
#21249 = CARTESIAN_POINT('Origin',(-6.44211288600659,0.755,8.59935470490582)) ;
#21250 = CARTESIAN_POINT('',(-6.46142056340518,0.748322417254363,8.55371893513969)) ;
#21251 = CARTESIAN_POINT('Origin',(-6.44211288600659,0.755,8.59935470490582)) ;
#21252 = CARTESIAN_POINT('Origin',(-6.44211288600659,0.755,8.59935470490582)) ;
#21253 = CARTESIAN_POINT('Origin',(-6.1946255125913,0.74,8.49684207832111)) ;
#21254 = CARTESIAN_POINT('',(-6.19765041936679,0.690091584487187,8.49684207832111)) ;
#21255 = CARTESIAN_POINT('',(-6.21393318998988,0.733322417254363,8.45120630855498)) ;
#21256 = CARTESIAN_POINT('Origin',(-6.1946255125913,0.74,8.49684207832111)) ;
#21257 = CARTESIAN_POINT('',(-6.21375968420955,0.74,8.45064810169555)) ;
#21258 = CARTESIAN_POINT('Origin',(-6.1946255125913,0.74,8.49684207832111)) ;
#21259 = CARTESIAN_POINT('',(-6.1946255125913,0.74,8.44684207832111)) ;
#21260 = CARTESIAN_POINT('Origin',(-6.1946255125913,0.74,8.49684207832111)) ;
#21261 = CARTESIAN_POINT('',(-6.19160060581581,0.789908415512813,8.49684207832111)) ;
#21262 = CARTESIAN_POINT('Origin',(-6.1946255125913,0.74,8.49684207832111)) ;
#21263 = CARTESIAN_POINT('Origin',(-6.1946255125913,0.74,8.49684207832111)) ;
#21264 = CARTESIAN_POINT('Origin',(-5.94713813917601,0.725,8.59935470490582)) ;
#21265 = CARTESIAN_POINT('',(-5.94927707126941,0.675091584487187,8.59721577281241)) ;
#21266 = CARTESIAN_POINT('',(-5.9449992070826,0.774908415512813,8.60149363699922)) ;
#21267 = CARTESIAN_POINT('Origin',(-5.94713813917601,0.725,8.59935470490582)) ;
#21268 = CARTESIAN_POINT('Origin',(-5.94713813917601,0.725,8.59935470490582)) ;
#21269 = CARTESIAN_POINT('Origin',(-5.8446255125913,0.71,8.84684207832111)) ;
#21270 = CARTESIAN_POINT('',(-5.8446255125913,0.660091584487187,8.84381717154562)) ;
#21271 = CARTESIAN_POINT('',(-5.8446255125913,0.759908415512813,8.8498669850966)) ;
#21272 = CARTESIAN_POINT('Origin',(-5.8446255125913,0.71,8.84684207832111)) ;
#21273 = CARTESIAN_POINT('Origin',(-5.8446255125913,0.71,8.84684207832111)) ;
#21274 = CARTESIAN_POINT('Origin',(-5.94713813917601,0.695,9.0943294517364)) ;
#21275 = CARTESIAN_POINT('',(-5.9449992070826,0.645091584487187,9.092190519643)) ;
#21276 = CARTESIAN_POINT('',(-5.94927707126941,0.744908415512813,9.09646838382981)) ;
#21277 = CARTESIAN_POINT('Origin',(-5.94713813917601,0.695,9.0943294517364)) ;
#21278 = CARTESIAN_POINT('Origin',(-5.94713813917601,0.695,9.0943294517364)) ;
#21279 = CARTESIAN_POINT('Origin',(-6.1946255125913,0.68,9.19684207832111)) ;
#21280 = CARTESIAN_POINT('',(-6.19160060581581,0.630091584487187,9.19684207832111)) ;
#21281 = CARTESIAN_POINT('',(-6.19765041936679,0.729908415512813,9.19684207832111)) ;
#21282 = CARTESIAN_POINT('Origin',(-6.1946255125913,0.68,9.19684207832111)) ;
#21283 = CARTESIAN_POINT('',(-6.21393318998988,0.686677582745637,9.24247784808724)) ;
#21284 = CARTESIAN_POINT('Origin',(-6.1946255125913,0.68,9.19684207832111)) ;
#21285 = CARTESIAN_POINT('',(-6.21375968420955,0.68,9.24303605494667)) ;
#21286 = CARTESIAN_POINT('Origin',(-6.1946255125913,0.68,9.19684207832111)) ;
#21287 = CARTESIAN_POINT('',(-6.1946255125913,0.68,9.24684207832111)) ;
#21288 = CARTESIAN_POINT('Origin',(-6.1946255125913,0.68,9.19684207832111)) ;
#21289 = CARTESIAN_POINT('Origin',(-6.1946255125913,0.68,9.19684207832111)) ;
#21290 = CARTESIAN_POINT('Origin',(-6.44211288600659,0.665,9.0943294517364)) ;
#21291 = CARTESIAN_POINT('',(-6.43997395391319,0.615091584487187,9.09646838382981)) ;
#21292 = CARTESIAN_POINT('',(-6.46142056340518,0.671677582745637,9.13996522150253)) ;
#21293 = CARTESIAN_POINT('Origin',(-6.44211288600659,0.665,9.0943294517364)) ;
#21294 = CARTESIAN_POINT('',(-6.4442518181,0.714908415512813,9.092190519643)) ;
#21295 = CARTESIAN_POINT('Origin',(-6.44211288600659,0.665,9.0943294517364)) ;
#21296 = CARTESIAN_POINT('',(-6.48831924755442,0.666155771164016,9.11339870304649)) ;
#21297 = CARTESIAN_POINT('Origin',(-6.44211288600659,0.665,9.0943294517364)) ;
#21298 = CARTESIAN_POINT('Origin',(-6.44211288600659,0.665,9.0943294517364)) ;
#21299 = CARTESIAN_POINT('Origin',(-6.5446255125913,0.65,8.84684207832111)) ;
#21300 = CARTESIAN_POINT('',(-6.5446255125913,0.600091584487187,8.8498669850966)) ;
#21301 = CARTESIAN_POINT('',(-6.59083187413913,0.651155771164016,8.8659113296312)) ;
#21302 = CARTESIAN_POINT('Origin',(-6.5446255125913,0.65,8.84684207832111)) ;
#21303 = CARTESIAN_POINT('',(-6.5446255125913,0.699908415512813,8.84381717154562)) ;
#21304 = CARTESIAN_POINT('Origin',(-6.5446255125913,0.65,8.84684207832111)) ;
#21305 = CARTESIAN_POINT('',(-6.59083187413913,0.648844228835984,8.82777282701102)) ;
#21306 = CARTESIAN_POINT('Origin',(-6.5446255125913,0.65,8.84684207832111)) ;
#21307 = CARTESIAN_POINT('Origin',(-6.5446255125913,0.65,8.84684207832111)) ;
#21308 = CARTESIAN_POINT('Origin',(-6.44211288600659,0.635,8.59935470490582)) ;
#21309 = CARTESIAN_POINT('',(-6.4442518181,0.585091584487187,8.60149363699922)) ;
#21310 = CARTESIAN_POINT('',(-6.48831924755442,0.633844228835984,8.58028545359573)) ;
#21311 = CARTESIAN_POINT('Origin',(-6.44211288600659,0.635,8.59935470490582)) ;
#21312 = CARTESIAN_POINT('',(-6.43997395391318,0.684908415512813,8.59721577281241)) ;
#21313 = CARTESIAN_POINT('Origin',(-6.44211288600659,0.635,8.59935470490582)) ;
#21314 = CARTESIAN_POINT('',(-6.46142056340518,0.628322417254363,8.55371893513969)) ;
#21315 = CARTESIAN_POINT('Origin',(-6.44211288600659,0.635,8.59935470490582)) ;
#21316 = CARTESIAN_POINT('Origin',(-6.44211288600659,0.635,8.59935470490582)) ;
#21317 = CARTESIAN_POINT('Origin',(-6.1946255125913,0.62,8.49684207832111)) ;
#21318 = CARTESIAN_POINT('',(-6.19765041936679,0.570091584487187,8.49684207832111)) ;
#21319 = CARTESIAN_POINT('',(-6.21393318998988,0.613322417254363,8.45120630855498)) ;
#21320 = CARTESIAN_POINT('Origin',(-6.1946255125913,0.62,8.49684207832111)) ;
#21321 = CARTESIAN_POINT('',(-6.21375968420955,0.62,8.45064810169555)) ;
#21322 = CARTESIAN_POINT('Origin',(-6.1946255125913,0.62,8.49684207832111)) ;
#21323 = CARTESIAN_POINT('',(-6.1946255125913,0.62,8.44684207832111)) ;
#21324 = CARTESIAN_POINT('Origin',(-6.1946255125913,0.62,8.49684207832111)) ;
#21325 = CARTESIAN_POINT('',(-6.19160060581581,0.669908415512813,8.49684207832111)) ;
#21326 = CARTESIAN_POINT('Origin',(-6.1946255125913,0.62,8.49684207832111)) ;
#21327 = CARTESIAN_POINT('Origin',(-6.1946255125913,0.62,8.49684207832111)) ;
#21328 = CARTESIAN_POINT('Origin',(-5.94713813917601,0.605,8.59935470490582)) ;
#21329 = CARTESIAN_POINT('',(-5.94927707126941,0.555091584487187,8.59721577281241)) ;
#21330 = CARTESIAN_POINT('',(-5.9449992070826,0.654908415512813,8.60149363699922)) ;
#21331 = CARTESIAN_POINT('Origin',(-5.94713813917601,0.605,8.59935470490582)) ;
#21332 = CARTESIAN_POINT('Origin',(-5.94713813917601,0.605,8.59935470490582)) ;
#21333 = CARTESIAN_POINT('Origin',(-5.8446255125913,0.59,8.84684207832111)) ;
#21334 = CARTESIAN_POINT('',(-5.8446255125913,0.540091584487187,8.84381717154562)) ;
#21335 = CARTESIAN_POINT('',(-5.8446255125913,0.639908415512813,8.8498669850966)) ;
#21336 = CARTESIAN_POINT('Origin',(-5.8446255125913,0.59,8.84684207832111)) ;
#21337 = CARTESIAN_POINT('Origin',(-5.8446255125913,0.59,8.84684207832111)) ;
#21338 = CARTESIAN_POINT('Origin',(-5.94713813917601,0.575,9.0943294517364)) ;
#21339 = CARTESIAN_POINT('',(-5.9449992070826,0.525091584487187,9.092190519643)) ;
#21340 = CARTESIAN_POINT('',(-5.94927707126941,0.624908415512813,9.09646838382981)) ;
#21341 = CARTESIAN_POINT('Origin',(-5.94713813917601,0.575,9.0943294517364)) ;
#21342 = CARTESIAN_POINT('Origin',(-5.94713813917601,0.575,9.0943294517364)) ;
#21343 = CARTESIAN_POINT('Origin',(-6.1946255125913,0.56,9.19684207832111)) ;
#21344 = CARTESIAN_POINT('',(-6.19160060581581,0.510091584487187,9.19684207832111)) ;
#21345 = CARTESIAN_POINT('',(-6.19765041936679,0.609908415512813,9.19684207832111)) ;
#21346 = CARTESIAN_POINT('Origin',(-6.1946255125913,0.56,9.19684207832111)) ;
#21347 = CARTESIAN_POINT('',(-6.21393318998988,0.566677582745637,9.24247784808724)) ;
#21348 = CARTESIAN_POINT('Origin',(-6.1946255125913,0.56,9.19684207832111)) ;
#21349 = CARTESIAN_POINT('',(-6.21375968420955,0.56,9.24303605494667)) ;
#21350 = CARTESIAN_POINT('Origin',(-6.1946255125913,0.56,9.19684207832111)) ;
#21351 = CARTESIAN_POINT('',(-6.1946255125913,0.56,9.24684207832111)) ;
#21352 = CARTESIAN_POINT('Origin',(-6.1946255125913,0.56,9.19684207832111)) ;
#21353 = CARTESIAN_POINT('Origin',(-6.1946255125913,0.56,9.19684207832111)) ;
#21354 = CARTESIAN_POINT('Origin',(-6.44211288600659,0.545,9.0943294517364)) ;
#21355 = CARTESIAN_POINT('',(-6.43997395391318,0.495091584487187,9.09646838382981)) ;
#21356 = CARTESIAN_POINT('',(-6.46142056340518,0.551677582745637,9.13996522150253)) ;
#21357 = CARTESIAN_POINT('Origin',(-6.44211288600659,0.545,9.0943294517364)) ;
#21358 = CARTESIAN_POINT('',(-6.4442518181,0.594908415512813,9.09219051964299)) ;
#21359 = CARTESIAN_POINT('Origin',(-6.44211288600659,0.545,9.0943294517364)) ;
#21360 = CARTESIAN_POINT('',(-6.48831924755442,0.546155771164016,9.11339870304649)) ;
#21361 = CARTESIAN_POINT('Origin',(-6.44211288600659,0.545,9.0943294517364)) ;
#21362 = CARTESIAN_POINT('Origin',(-6.44211288600659,0.545,9.0943294517364)) ;
#21363 = CARTESIAN_POINT('Origin',(-6.5446255125913,0.53,8.84684207832111)) ;
#21364 = CARTESIAN_POINT('',(-6.5446255125913,0.480091584487187,8.8498669850966)) ;
#21365 = CARTESIAN_POINT('',(-6.59083187413913,0.531155771164016,8.8659113296312)) ;
#21366 = CARTESIAN_POINT('Origin',(-6.5446255125913,0.53,8.84684207832111)) ;
#21367 = CARTESIAN_POINT('',(-6.5446255125913,0.579908415512813,8.84381717154562)) ;
#21368 = CARTESIAN_POINT('Origin',(-6.5446255125913,0.53,8.84684207832111)) ;
#21369 = CARTESIAN_POINT('',(-6.59083187413913,0.528844228835984,8.82777282701102)) ;
#21370 = CARTESIAN_POINT('Origin',(-6.5446255125913,0.53,8.84684207832111)) ;
#21371 = CARTESIAN_POINT('Origin',(-6.5446255125913,0.53,8.84684207832111)) ;
#21372 = CARTESIAN_POINT('Origin',(-6.44211288600659,0.515,8.59935470490582)) ;
#21373 = CARTESIAN_POINT('',(-6.4442518181,0.465091584487187,8.60149363699922)) ;
#21374 = CARTESIAN_POINT('',(-6.48831924755442,0.513844228835984,8.58028545359573)) ;
#21375 = CARTESIAN_POINT('Origin',(-6.44211288600659,0.515,8.59935470490582)) ;
#21376 = CARTESIAN_POINT('',(-6.43997395391318,0.564908415512813,8.59721577281241)) ;
#21377 = CARTESIAN_POINT('Origin',(-6.44211288600659,0.515,8.59935470490582)) ;
#21378 = CARTESIAN_POINT('',(-6.46142056340518,0.508322417254363,8.55371893513969)) ;
#21379 = CARTESIAN_POINT('Origin',(-6.44211288600659,0.515,8.59935470490582)) ;
#21380 = CARTESIAN_POINT('Origin',(-6.44211288600659,0.515,8.59935470490582)) ;
#21381 = CARTESIAN_POINT('Origin',(-6.1946255125913,0.5,8.49684207832111)) ;
#21382 = CARTESIAN_POINT('',(-6.19765041936679,0.450091584487187,8.49684207832111)) ;
#21383 = CARTESIAN_POINT('',(-6.21393318998988,0.493322417254363,8.45120630855498)) ;
#21384 = CARTESIAN_POINT('Origin',(-6.1946255125913,0.5,8.49684207832111)) ;
#21385 = CARTESIAN_POINT('',(-6.21375968420955,0.5,8.45064810169555)) ;
#21386 = CARTESIAN_POINT('Origin',(-6.1946255125913,0.5,8.49684207832111)) ;
#21387 = CARTESIAN_POINT('',(-6.1946255125913,0.5,8.44684207832111)) ;
#21388 = CARTESIAN_POINT('Origin',(-6.1946255125913,0.5,8.49684207832111)) ;
#21389 = CARTESIAN_POINT('',(-6.19160060581581,0.549908415512813,8.49684207832111)) ;
#21390 = CARTESIAN_POINT('Origin',(-6.1946255125913,0.5,8.49684207832111)) ;
#21391 = CARTESIAN_POINT('Origin',(-6.1946255125913,0.5,8.49684207832111)) ;
#21392 = CARTESIAN_POINT('Origin',(-5.94713813917601,0.485,8.59935470490582)) ;
#21393 = CARTESIAN_POINT('',(-5.94927707126941,0.435091584487187,8.59721577281241)) ;
#21394 = CARTESIAN_POINT('',(-5.9449992070826,0.534908415512813,8.60149363699922)) ;
#21395 = CARTESIAN_POINT('Origin',(-5.94713813917601,0.485,8.59935470490582)) ;
#21396 = CARTESIAN_POINT('Origin',(-5.94713813917601,0.485,8.59935470490582)) ;
#21397 = CARTESIAN_POINT('Origin',(-5.8446255125913,0.47,8.84684207832111)) ;
#21398 = CARTESIAN_POINT('',(-5.8446255125913,0.420091584487187,8.84381717154562)) ;
#21399 = CARTESIAN_POINT('',(-5.8446255125913,0.519908415512813,8.8498669850966)) ;
#21400 = CARTESIAN_POINT('Origin',(-5.8446255125913,0.47,8.84684207832111)) ;
#21401 = CARTESIAN_POINT('Origin',(-5.8446255125913,0.47,8.84684207832111)) ;
#21402 = CARTESIAN_POINT('Origin',(-5.94713813917601,0.455,9.0943294517364)) ;
#21403 = CARTESIAN_POINT('',(-5.9449992070826,0.405091584487187,9.092190519643)) ;
#21404 = CARTESIAN_POINT('',(-5.94927707126941,0.504908415512813,9.09646838382981)) ;
#21405 = CARTESIAN_POINT('Origin',(-5.94713813917601,0.455,9.0943294517364)) ;
#21406 = CARTESIAN_POINT('Origin',(-5.94713813917601,0.455,9.0943294517364)) ;
#21407 = CARTESIAN_POINT('Origin',(-6.1946255125913,0.44,9.19684207832111)) ;
#21408 = CARTESIAN_POINT('',(-6.19160060581581,0.390091584487187,9.19684207832111)) ;
#21409 = CARTESIAN_POINT('',(-6.19765041936679,0.489908415512813,9.19684207832111)) ;
#21410 = CARTESIAN_POINT('Origin',(-6.1946255125913,0.44,9.19684207832111)) ;
#21411 = CARTESIAN_POINT('',(-6.21393318998988,0.446677582745637,9.24247784808724)) ;
#21412 = CARTESIAN_POINT('Origin',(-6.1946255125913,0.44,9.19684207832111)) ;
#21413 = CARTESIAN_POINT('',(-6.21375968420955,0.44,9.24303605494667)) ;
#21414 = CARTESIAN_POINT('Origin',(-6.1946255125913,0.44,9.19684207832111)) ;
#21415 = CARTESIAN_POINT('',(-6.1946255125913,0.44,9.24684207832111)) ;
#21416 = CARTESIAN_POINT('Origin',(-6.1946255125913,0.44,9.19684207832111)) ;
#21417 = CARTESIAN_POINT('Origin',(-6.1946255125913,0.44,9.19684207832111)) ;
#21418 = CARTESIAN_POINT('Origin',(-6.44211288600659,0.425,9.0943294517364)) ;
#21419 = CARTESIAN_POINT('',(-6.43997395391318,0.375091584487187,9.09646838382981)) ;
#21420 = CARTESIAN_POINT('',(-6.46142056340518,0.431677582745637,9.13996522150253)) ;
#21421 = CARTESIAN_POINT('Origin',(-6.44211288600659,0.425,9.0943294517364)) ;
#21422 = CARTESIAN_POINT('',(-6.4442518181,0.474908415512813,9.09219051964299)) ;
#21423 = CARTESIAN_POINT('Origin',(-6.44211288600659,0.425,9.0943294517364)) ;
#21424 = CARTESIAN_POINT('',(-6.48831924755442,0.426155771164016,9.1133987030465)) ;
#21425 = CARTESIAN_POINT('Origin',(-6.44211288600659,0.425,9.0943294517364)) ;
#21426 = CARTESIAN_POINT('Origin',(-6.44211288600659,0.425,9.0943294517364)) ;
#21427 = CARTESIAN_POINT('Origin',(-6.5446255125913,0.41,8.84684207832111)) ;
#21428 = CARTESIAN_POINT('',(-6.5446255125913,0.360091584487187,8.8498669850966)) ;
#21429 = CARTESIAN_POINT('',(-6.59083187413913,0.411155771164016,8.8659113296312)) ;
#21430 = CARTESIAN_POINT('Origin',(-6.5446255125913,0.41,8.84684207832111)) ;
#21431 = CARTESIAN_POINT('',(-6.5446255125913,0.459908415512813,8.84381717154562)) ;
#21432 = CARTESIAN_POINT('Origin',(-6.5446255125913,0.41,8.84684207832111)) ;
#21433 = CARTESIAN_POINT('',(-6.59083187413913,0.408844228835984,8.82777282701102)) ;
#21434 = CARTESIAN_POINT('Origin',(-6.5446255125913,0.41,8.84684207832111)) ;
#21435 = CARTESIAN_POINT('Origin',(-6.5446255125913,0.41,8.84684207832111)) ;
#21436 = CARTESIAN_POINT('Origin',(-6.44211288600659,0.395,8.59935470490582)) ;
#21437 = CARTESIAN_POINT('',(-6.4442518181,0.345091584487187,8.60149363699923)) ;
#21438 = CARTESIAN_POINT('',(-6.48831924755442,0.393844228835984,8.58028545359573)) ;
#21439 = CARTESIAN_POINT('Origin',(-6.44211288600659,0.395,8.59935470490582)) ;
#21440 = CARTESIAN_POINT('',(-6.43997395391318,0.444908415512813,8.59721577281242)) ;
#21441 = CARTESIAN_POINT('Origin',(-6.44211288600659,0.395,8.59935470490582)) ;
#21442 = CARTESIAN_POINT('',(-6.46142056340518,0.388322417254363,8.55371893513969)) ;
#21443 = CARTESIAN_POINT('Origin',(-6.44211288600659,0.395,8.59935470490582)) ;
#21444 = CARTESIAN_POINT('Origin',(-6.44211288600659,0.395,8.59935470490582)) ;
#21445 = CARTESIAN_POINT('Origin',(-6.1946255125913,0.38,8.49684207832111)) ;
#21446 = CARTESIAN_POINT('',(-6.19765041936679,0.330091584487187,8.49684207832111)) ;
#21447 = CARTESIAN_POINT('',(-6.21393318998988,0.373322417254363,8.45120630855498)) ;
#21448 = CARTESIAN_POINT('Origin',(-6.1946255125913,0.38,8.49684207832111)) ;
#21449 = CARTESIAN_POINT('',(-6.21375968420955,0.38,8.45064810169555)) ;
#21450 = CARTESIAN_POINT('Origin',(-6.1946255125913,0.38,8.49684207832111)) ;
#21451 = CARTESIAN_POINT('',(-6.1946255125913,0.38,8.44684207832111)) ;
#21452 = CARTESIAN_POINT('Origin',(-6.1946255125913,0.38,8.49684207832111)) ;
#21453 = CARTESIAN_POINT('',(-6.19160060581581,0.429908415512813,8.49684207832111)) ;
#21454 = CARTESIAN_POINT('Origin',(-6.1946255125913,0.38,8.49684207832111)) ;
#21455 = CARTESIAN_POINT('Origin',(-6.1946255125913,0.38,8.49684207832111)) ;
#21456 = CARTESIAN_POINT('Origin',(-5.94713813917601,0.365,8.59935470490582)) ;
#21457 = CARTESIAN_POINT('',(-5.94927707126941,0.315091584487187,8.59721577281241)) ;
#21458 = CARTESIAN_POINT('',(-5.9449992070826,0.414908415512813,8.60149363699922)) ;
#21459 = CARTESIAN_POINT('Origin',(-5.94713813917601,0.365,8.59935470490582)) ;
#21460 = CARTESIAN_POINT('Origin',(-5.94713813917601,0.365,8.59935470490582)) ;
#21461 = CARTESIAN_POINT('Origin',(-5.89588182588365,0.8225,8.97058576502876)) ;
#21462 = CARTESIAN_POINT('',(-5.89083187413913,0.831155771164016,8.82777282701102)) ;
#21463 = CARTESIAN_POINT('Origin',(-5.8446255125913,0.83,8.84684207832111)) ;
#21464 = CARTESIAN_POINT('',(-5.98545422562987,0.817310303345588,9.05621139128359)) ;
#21465 = CARTESIAN_POINT('',(-5.94208818743149,0.823655771164016,8.95151651371867)) ;
#21466 = CARTESIAN_POINT('',(-5.98539769271865,0.820528925590979,9.05654380610156)) ;
#21467 = CARTESIAN_POINT('Origin',(-5.94713813917601,0.815,9.0943294517364)) ;
#21468 = CARTESIAN_POINT('Origin',(-5.94713813917601,0.815,9.0943294517364)) ;
#21469 = CARTESIAN_POINT('Origin',(-5.94713813917601,0.815,9.0943294517364)) ;
#21470 = CARTESIAN_POINT('Origin',(-5.8446255125913,0.83,8.84684207832111)) ;
#21471 = CARTESIAN_POINT('Origin',(-6.07088182588365,0.8075,9.14558576502876)) ;
#21472 = CARTESIAN_POINT('',(-6.1950994204991,0.807819081556115,9.14340510580129)) ;
#21473 = CARTESIAN_POINT('',(-6.09018950328224,0.814177582745637,9.09994999526262)) ;
#21474 = CARTESIAN_POINT('Origin',(-6.1946255125913,0.8,9.19684207832111)) ;
#21475 = CARTESIAN_POINT('Origin',(-6.1946255125913,0.8,9.19684207832111)) ;
#21476 = CARTESIAN_POINT('Origin',(-6.31836919929895,0.7925,9.14558576502876)) ;
#21477 = CARTESIAN_POINT('',(-6.33767687669753,0.799177582745637,9.19122153479489)) ;
#21478 = CARTESIAN_POINT('Origin',(-6.44211288600659,0.785,9.0943294517364)) ;
#21479 = CARTESIAN_POINT('Origin',(-6.49336919929894,0.7775,8.97058576502876)) ;
#21480 = CARTESIAN_POINT('',(-6.53957556084678,0.778655771164016,8.98965501633885)) ;
#21481 = CARTESIAN_POINT('Origin',(-6.5446255125913,0.77,8.84684207832111)) ;
#21482 = CARTESIAN_POINT('Origin',(-6.49336919929894,0.7625,8.72309839161347)) ;
#21483 = CARTESIAN_POINT('',(-6.53957556084678,0.761344228835984,8.70402914030337)) ;
#21484 = CARTESIAN_POINT('Origin',(-6.44211288600659,0.755,8.59935470490582)) ;
#21485 = CARTESIAN_POINT('Origin',(-6.31836919929894,0.7475,8.54809839161346)) ;
#21486 = CARTESIAN_POINT('',(-6.33767687669753,0.740822417254363,8.50246262184733)) ;
#21487 = CARTESIAN_POINT('',(-6.1950994204991,0.732180918443886,8.55027905084093)) ;
#21488 = CARTESIAN_POINT('Origin',(-6.1946255125913,0.74,8.49684207832111)) ;
#21489 = CARTESIAN_POINT('Origin',(-6.1946255125913,0.74,8.49684207832111)) ;
#21490 = CARTESIAN_POINT('Origin',(-6.07088182588365,0.7325,8.54809839161346)) ;
#21491 = CARTESIAN_POINT('',(-5.98539769271865,0.719471074409021,8.63714035054067)) ;
#21492 = CARTESIAN_POINT('',(-6.09018950328224,0.725822417254363,8.5937341613796)) ;
#21493 = CARTESIAN_POINT('',(-5.98545422562987,0.722689696654412,8.63747276535863)) ;
#21494 = CARTESIAN_POINT('Origin',(-5.94713813917601,0.725,8.59935470490582)) ;
#21495 = CARTESIAN_POINT('Origin',(-5.94713813917601,0.725,8.59935470490582)) ;
#21496 = CARTESIAN_POINT('Origin',(-5.94713813917601,0.725,8.59935470490582)) ;
#21497 = CARTESIAN_POINT('Origin',(-5.89588182588365,0.7175,8.72309839161347)) ;
#21498 = CARTESIAN_POINT('',(-5.89873061665607,0.71,8.84684207832111)) ;
#21499 = CARTESIAN_POINT('',(-5.94208818743149,0.716344228835984,8.74216764292356)) ;
#21500 = CARTESIAN_POINT('Origin',(-5.8446255125913,0.71,8.84684207832111)) ;
#21501 = CARTESIAN_POINT('Origin',(-5.8446255125913,0.71,8.84684207832111)) ;
#21502 = CARTESIAN_POINT('Origin',(-5.89588182588365,0.7025,8.97058576502876)) ;
#21503 = CARTESIAN_POINT('',(-5.98545422562987,0.697310303345588,9.05621139128359)) ;
#21504 = CARTESIAN_POINT('',(-5.94208818743149,0.703655771164016,8.95151651371867)) ;
#21505 = CARTESIAN_POINT('',(-5.98539769271865,0.700528925590979,9.05654380610155)) ;
#21506 = CARTESIAN_POINT('Origin',(-5.94713813917601,0.695,9.0943294517364)) ;
#21507 = CARTESIAN_POINT('Origin',(-5.94713813917601,0.695,9.0943294517364)) ;
#21508 = CARTESIAN_POINT('Origin',(-5.94713813917601,0.695,9.0943294517364)) ;
#21509 = CARTESIAN_POINT('Origin',(-6.07088182588365,0.6875,9.14558576502876)) ;
#21510 = CARTESIAN_POINT('',(-6.1950994204991,0.687819081556115,9.14340510580129)) ;
#21511 = CARTESIAN_POINT('',(-6.09018950328224,0.694177582745637,9.09994999526262)) ;
#21512 = CARTESIAN_POINT('Origin',(-6.1946255125913,0.68,9.19684207832111)) ;
#21513 = CARTESIAN_POINT('Origin',(-6.1946255125913,0.68,9.19684207832111)) ;
#21514 = CARTESIAN_POINT('Origin',(-6.31836919929895,0.6725,9.14558576502876)) ;
#21515 = CARTESIAN_POINT('',(-6.33767687669753,0.679177582745637,9.19122153479489)) ;
#21516 = CARTESIAN_POINT('Origin',(-6.44211288600659,0.665,9.0943294517364)) ;
#21517 = CARTESIAN_POINT('Origin',(-6.49336919929894,0.6575,8.97058576502876)) ;
#21518 = CARTESIAN_POINT('',(-6.53957556084678,0.658655771164016,8.98965501633885)) ;
#21519 = CARTESIAN_POINT('Origin',(-6.5446255125913,0.65,8.84684207832111)) ;
#21520 = CARTESIAN_POINT('Origin',(-6.49336919929894,0.6425,8.72309839161347)) ;
#21521 = CARTESIAN_POINT('',(-6.53957556084678,0.641344228835984,8.70402914030337)) ;
#21522 = CARTESIAN_POINT('Origin',(-6.44211288600659,0.635,8.59935470490582)) ;
#21523 = CARTESIAN_POINT('Origin',(-6.31836919929894,0.6275,8.54809839161346)) ;
#21524 = CARTESIAN_POINT('',(-6.33767687669753,0.620822417254363,8.50246262184733)) ;
#21525 = CARTESIAN_POINT('',(-6.1950994204991,0.612180918443886,8.55027905084093)) ;
#21526 = CARTESIAN_POINT('Origin',(-6.1946255125913,0.62,8.49684207832111)) ;
#21527 = CARTESIAN_POINT('Origin',(-6.1946255125913,0.62,8.49684207832111)) ;
#21528 = CARTESIAN_POINT('Origin',(-6.07088182588365,0.6125,8.54809839161346)) ;
#21529 = CARTESIAN_POINT('',(-5.98539769271865,0.599471074409021,8.63714035054067)) ;
#21530 = CARTESIAN_POINT('',(-6.09018950328224,0.605822417254363,8.5937341613796)) ;
#21531 = CARTESIAN_POINT('',(-5.98545422562987,0.602689696654412,8.63747276535863)) ;
#21532 = CARTESIAN_POINT('Origin',(-5.94713813917601,0.605,8.59935470490582)) ;
#21533 = CARTESIAN_POINT('Origin',(-5.94713813917601,0.605,8.59935470490582)) ;
#21534 = CARTESIAN_POINT('Origin',(-5.94713813917601,0.605,8.59935470490582)) ;
#21535 = CARTESIAN_POINT('Origin',(-5.89588182588365,0.5975,8.72309839161347)) ;
#21536 = CARTESIAN_POINT('',(-5.89873061665607,0.59,8.84684207832111)) ;
#21537 = CARTESIAN_POINT('',(-5.94208818743149,0.596344228835984,8.74216764292356)) ;
#21538 = CARTESIAN_POINT('Origin',(-5.8446255125913,0.59,8.84684207832111)) ;
#21539 = CARTESIAN_POINT('Origin',(-5.8446255125913,0.59,8.84684207832111)) ;
#21540 = CARTESIAN_POINT('Origin',(-5.89588182588365,0.5825,8.97058576502876)) ;
#21541 = CARTESIAN_POINT('',(-5.98545422562987,0.577310303345588,9.05621139128359)) ;
#21542 = CARTESIAN_POINT('',(-5.94208818743149,0.583655771164016,8.95151651371867)) ;
#21543 = CARTESIAN_POINT('',(-5.98539769271865,0.58052892559098,9.05654380610155)) ;
#21544 = CARTESIAN_POINT('Origin',(-5.94713813917601,0.575,9.0943294517364)) ;
#21545 = CARTESIAN_POINT('Origin',(-5.94713813917601,0.575,9.0943294517364)) ;
#21546 = CARTESIAN_POINT('Origin',(-5.94713813917601,0.575,9.0943294517364)) ;
#21547 = CARTESIAN_POINT('Origin',(-6.07088182588365,0.5675,9.14558576502876)) ;
#21548 = CARTESIAN_POINT('',(-6.1950994204991,0.567819081556115,9.14340510580128)) ;
#21549 = CARTESIAN_POINT('',(-6.09018950328224,0.574177582745637,9.09994999526262)) ;
#21550 = CARTESIAN_POINT('Origin',(-6.1946255125913,0.56,9.19684207832111)) ;
#21551 = CARTESIAN_POINT('Origin',(-6.1946255125913,0.56,9.19684207832111)) ;
#21552 = CARTESIAN_POINT('Origin',(-6.31836919929894,0.5525,9.14558576502876)) ;
#21553 = CARTESIAN_POINT('',(-6.33767687669753,0.559177582745637,9.19122153479489)) ;
#21554 = CARTESIAN_POINT('Origin',(-6.44211288600659,0.545,9.0943294517364)) ;
#21555 = CARTESIAN_POINT('Origin',(-6.49336919929894,0.5375,8.97058576502876)) ;
#21556 = CARTESIAN_POINT('',(-6.53957556084678,0.538655771164016,8.98965501633885)) ;
#21557 = CARTESIAN_POINT('Origin',(-6.5446255125913,0.53,8.84684207832111)) ;
#21558 = CARTESIAN_POINT('Origin',(-6.49336919929894,0.5225,8.72309839161347)) ;
#21559 = CARTESIAN_POINT('',(-6.53957556084678,0.521344228835984,8.70402914030337)) ;
#21560 = CARTESIAN_POINT('Origin',(-6.44211288600659,0.515,8.59935470490582)) ;
#21561 = CARTESIAN_POINT('Origin',(-6.31836919929894,0.5075,8.54809839161346)) ;
#21562 = CARTESIAN_POINT('',(-6.33767687669753,0.500822417254363,8.50246262184733)) ;
#21563 = CARTESIAN_POINT('',(-6.1950994204991,0.492180918443886,8.55027905084093)) ;
#21564 = CARTESIAN_POINT('Origin',(-6.1946255125913,0.5,8.49684207832111)) ;
#21565 = CARTESIAN_POINT('Origin',(-6.1946255125913,0.5,8.49684207832111)) ;
#21566 = CARTESIAN_POINT('Origin',(-6.07088182588365,0.4925,8.54809839161346)) ;
#21567 = CARTESIAN_POINT('',(-5.98539769271865,0.47947107440902,8.63714035054067)) ;
#21568 = CARTESIAN_POINT('',(-6.09018950328224,0.485822417254363,8.5937341613796)) ;
#21569 = CARTESIAN_POINT('',(-5.98545422562987,0.482689696654412,8.63747276535863)) ;
#21570 = CARTESIAN_POINT('Origin',(-5.94713813917601,0.485,8.59935470490582)) ;
#21571 = CARTESIAN_POINT('Origin',(-5.94713813917601,0.485,8.59935470490582)) ;
#21572 = CARTESIAN_POINT('Origin',(-5.94713813917601,0.485,8.59935470490582)) ;
#21573 = CARTESIAN_POINT('Origin',(-5.89588182588365,0.4775,8.72309839161347)) ;
#21574 = CARTESIAN_POINT('',(-5.89873061665607,0.47,8.84684207832111)) ;
#21575 = CARTESIAN_POINT('',(-5.94208818743149,0.476344228835984,8.74216764292356)) ;
#21576 = CARTESIAN_POINT('Origin',(-5.8446255125913,0.47,8.84684207832111)) ;
#21577 = CARTESIAN_POINT('Origin',(-5.8446255125913,0.47,8.84684207832111)) ;
#21578 = CARTESIAN_POINT('Origin',(-5.89588182588365,0.4625,8.97058576502876)) ;
#21579 = CARTESIAN_POINT('',(-5.98545422562987,0.457310303345588,9.05621139128359)) ;
#21580 = CARTESIAN_POINT('',(-5.94208818743149,0.463655771164016,8.95151651371867)) ;
#21581 = CARTESIAN_POINT('',(-5.98539769271865,0.46052892559098,9.05654380610155)) ;
#21582 = CARTESIAN_POINT('Origin',(-5.94713813917601,0.455,9.0943294517364)) ;
#21583 = CARTESIAN_POINT('Origin',(-5.94713813917601,0.455,9.0943294517364)) ;
#21584 = CARTESIAN_POINT('Origin',(-5.94713813917601,0.455,9.0943294517364)) ;
#21585 = CARTESIAN_POINT('Origin',(-6.07088182588365,0.4475,9.14558576502876)) ;
#21586 = CARTESIAN_POINT('',(-6.1950994204991,0.447819081556115,9.14340510580128)) ;
#21587 = CARTESIAN_POINT('',(-6.09018950328224,0.454177582745637,9.09994999526262)) ;
#21588 = CARTESIAN_POINT('Origin',(-6.1946255125913,0.44,9.19684207832111)) ;
#21589 = CARTESIAN_POINT('Origin',(-6.1946255125913,0.44,9.19684207832111)) ;
#21590 = CARTESIAN_POINT('Origin',(-6.31836919929894,0.4325,9.14558576502876)) ;
#21591 = CARTESIAN_POINT('',(-6.33767687669753,0.439177582745637,9.19122153479489)) ;
#21592 = CARTESIAN_POINT('Origin',(-6.44211288600659,0.425,9.0943294517364)) ;
#21593 = CARTESIAN_POINT('Origin',(-6.49336919929894,0.4175,8.97058576502876)) ;
#21594 = CARTESIAN_POINT('',(-6.53957556084678,0.418655771164016,8.98965501633885)) ;
#21595 = CARTESIAN_POINT('Origin',(-6.5446255125913,0.41,8.84684207832111)) ;
#21596 = CARTESIAN_POINT('Origin',(-6.49336919929894,0.4025,8.72309839161347)) ;
#21597 = CARTESIAN_POINT('',(-6.53957556084678,0.401344228835984,8.70402914030337)) ;
#21598 = CARTESIAN_POINT('Origin',(-6.44211288600659,0.395,8.59935470490582)) ;
#21599 = CARTESIAN_POINT('Origin',(-6.31836919929894,0.3875,8.54809839161346)) ;
#21600 = CARTESIAN_POINT('',(-6.33767687669753,0.380822417254363,8.50246262184733)) ;
#21601 = CARTESIAN_POINT('',(-6.1950994204991,0.372180918443886,8.55027905084093)) ;
#21602 = CARTESIAN_POINT('Origin',(-6.1946255125913,0.38,8.49684207832111)) ;
#21603 = CARTESIAN_POINT('Origin',(-6.1946255125913,0.38,8.49684207832111)) ;
#21604 = CARTESIAN_POINT('Origin',(-6.07088182588365,0.3725,8.54809839161346)) ;
#21605 = CARTESIAN_POINT('',(-5.98539769271865,0.35947107440902,8.63714035054067)) ;
#21606 = CARTESIAN_POINT('',(-6.09018950328224,0.365822417254363,8.5937341613796)) ;
#21607 = CARTESIAN_POINT('',(-5.98545422562987,0.362689696654412,8.63747276535863)) ;
#21608 = CARTESIAN_POINT('Origin',(-5.94713813917601,0.365,8.59935470490582)) ;
#21609 = CARTESIAN_POINT('Origin',(-5.94713813917601,0.365,8.59935470490582)) ;
#21610 = CARTESIAN_POINT('Origin',(-5.94713813917601,0.365,8.59935470490582)) ;
#21611 = CARTESIAN_POINT('Origin',(-5.89588182588365,0.3575,8.72309839161347)) ;
#21612 = CARTESIAN_POINT('',(-5.89083187413913,0.348844228835984,8.8659113296312)) ;
#21613 = CARTESIAN_POINT('',(-5.94208818743149,0.356344228835984,8.74216764292356)) ;
#21614 = CARTESIAN_POINT('Origin',(-5.8446255125913,0.35,8.84684207832111)) ;
#21615 = CARTESIAN_POINT('Origin',(-5.8446255125913,0.35,8.84684207832111)) ;
#21616 = CARTESIAN_POINT('',(0.,0.,0.)) ;
#21617 = CARTESIAN_POINT('Origin',(-8.33803164073718,5.6,3.88808800801444)) ;
#21618 = CARTESIAN_POINT('',(-9.43554118180326,5.6,3.81410958366699)) ;
#21619 = CARTESIAN_POINT('Origin',(-8.49738695853213,5.6,3.46268140924831)) ;
#21620 = CARTESIAN_POINT('',(-8.33803164073718,5.6,4.98808800801443)) ;
#21621 = CARTESIAN_POINT('Origin',(-8.33803164073718,5.6,3.88808800801444)) ;
#21622 = CARTESIAN_POINT('Origin',(-8.84043936189492,5.6,2.54688670510862)) ;
#21623 = CARTESIAN_POINT('',(-8.84043936189492,5.6,3.94688670510862)) ;
#21624 = CARTESIAN_POINT('Origin',(-8.84043936189492,5.6,2.54688670510862)) ;
#21625 = CARTESIAN_POINT('Origin',(-8.33803164073718,5.6,3.88808800801444)) ;
#21626 = CARTESIAN_POINT('',(-9.37115550181876,5.6,3.51039092348254)) ;
#21627 = CARTESIAN_POINT('Origin',(-8.58923550131605,5.6,3.21748735656153)) ;
#21628 = CARTESIAN_POINT('',(-8.33803164073718,5.6,2.78808800801444)) ;
#21629 = CARTESIAN_POINT('Origin',(-8.33803164073718,5.6,3.88808800801444)) ;
#21630 = CARTESIAN_POINT('Origin',(-8.84043936189492,5.6,2.54688670510862)) ;
#21631 = CARTESIAN_POINT('',(-8.84043936189492,5.6,3.64688670510861)) ;
#21632 = CARTESIAN_POINT('Origin',(-8.84043936189492,5.6,2.54688670510862)) ;
#21633 = CARTESIAN_POINT('Origin',(-8.84043936189492,5.6,2.54688670510862)) ;
#21634 = CARTESIAN_POINT('',(-8.20946536255214,4.73397459621556,2.79562715648993)) ;
#21635 = CARTESIAN_POINT('',(-9.1527027256478,4.73397459621556,3.14895945125955)) ;
#21636 = CARTESIAN_POINT('Origin',(-8.68108404409997,5.6,2.97229330387474)) ;
#21637 = CARTESIAN_POINT('Ctrl Pts',(-9.1527027256478,4.73397459621556,3.14895945125955)) ;
#21638 = CARTESIAN_POINT('Ctrl Pts',(-9.13645723854168,4.71566855398674,3.13105359647328)) ;
#21639 = CARTESIAN_POINT('Ctrl Pts',(-9.1190870121684,4.69851255867057,3.11309468626371)) ;
#21640 = CARTESIAN_POINT('Ctrl Pts',(-9.05446121186005,4.64303800908893,3.05094049520305)) ;
#21641 = CARTESIAN_POINT('Ctrl Pts',(-8.99680270458556,4.6083948945016,3.00378876637968)) ;
#21642 = CARTESIAN_POINT('Ctrl Pts',(-8.86677648250724,4.56256392827545,2.92041371476685)) ;
#21643 = CARTESIAN_POINT('Ctrl Pts',(-8.79430324329648,4.55136544237033,2.88436092742056)) ;
#21644 = CARTESIAN_POINT('Ctrl Pts',(-8.65350061397982,4.55136544237033,2.83161692249397)) ;
#21645 = CARTESIAN_POINT('Ctrl Pts',(-8.57517702407941,4.56256392827545,2.81118192451869)) ;
#21646 = CARTESIAN_POINT('Ctrl Pts',(-8.42237405343921,4.6083948945016,2.78861048630727)) ;
#21647 = CARTESIAN_POINT('Ctrl Pts',(-8.34792716046905,4.64303800908893,2.78627615144598)) ;
#21648 = CARTESIAN_POINT('Ctrl Pts',(-8.25837107871867,4.69851255867057,2.79067453221843)) ;
#21649 = CARTESIAN_POINT('Ctrl Pts',(-8.23347682647838,4.71566855398674,2.79280136685503)) ;
#21650 = CARTESIAN_POINT('Ctrl Pts',(-8.20946536255214,4.73397459621556,2.79562715648993)) ;
#21651 = CARTESIAN_POINT('Origin',(-8.33803164073718,4.7,3.88808800801444)) ;
#21652 = CARTESIAN_POINT('Origin',(-8.33803164073718,4.73397459621556,3.88808800801444)) ;
#21653 = CARTESIAN_POINT('Origin',(-8.33803164073718,5.6,3.88808800801444)) ;
#21654 = CARTESIAN_POINT('Origin',(-9.12860070072158,5.6,1.14396208275687)) ;
#21655 = CARTESIAN_POINT('',(-9.91316825898094,5.6,2.30346790271938)) ;
#21656 = CARTESIAN_POINT('Origin',(-8.93183931414709,5.6,2.10190250279173)) ;
#21657 = CARTESIAN_POINT('',(-9.12860070072158,5.6,2.54396208275687)) ;
#21658 = CARTESIAN_POINT('Origin',(-9.12860070072158,5.6,1.14396208275687)) ;
#21659 = CARTESIAN_POINT('Origin',(-8.84043936189492,5.6,2.54688670510862)) ;
#21660 = CARTESIAN_POINT('',(-9.6192382673711,5.6,3.32372147829343)) ;
#21661 = CARTESIAN_POINT('Origin',(-8.84043936189492,5.6,2.54688670510862)) ;
#21662 = CARTESIAN_POINT('',(-7.74292982082884,5.6,2.62086512945606)) ;
#21663 = CARTESIAN_POINT('Ctrl Pts',(-7.74292982082884,5.6,2.62086512945606)) ;
#21664 = CARTESIAN_POINT('Ctrl Pts',(-7.74292982082884,5.47323659419775,2.62086512945606)) ;
#21665 = CARTESIAN_POINT('Ctrl Pts',(-7.76540878473659,5.33803946527454,2.60956776356783)) ;
#21666 = CARTESIAN_POINT('Ctrl Pts',(-7.85827962884553,5.08718469591568,2.57190072801271)) ;
#21667 = CARTESIAN_POINT('Ctrl Pts',(-7.92885376828481,4.97144567551952,2.54652928381717)) ;
#21668 = CARTESIAN_POINT('Ctrl Pts',(-8.04906993302529,4.83434481308716,2.5176859704715)) ;
#21669 = CARTESIAN_POINT('Ctrl Pts',(-8.09402492641871,4.79043643796436,2.50863906272968)) ;
#21670 = CARTESIAN_POINT('Ctrl Pts',(-8.19142307953697,4.711142531426,2.49491730637113)) ;
#21671 = CARTESIAN_POINT('Ctrl Pts',(-8.24386922105279,4.67574116355534,2.49035537389413)) ;
#21672 = CARTESIAN_POINT('Ctrl Pts',(-8.37274894896879,4.60209590056535,2.48630683631571)) ;
#21673 = CARTESIAN_POINT('Ctrl Pts',(-8.46381978450228,4.56343058934306,2.49058271315158)) ;
#21674 = CARTESIAN_POINT('Ctrl Pts',(-8.64959407180091,4.51264465486516,2.519960558875)) ;
#21675 = CARTESIAN_POINT('Ctrl Pts',(-8.7442527880297,4.50047177654324,2.54525472945496)) ;
#21676 = CARTESIAN_POINT('Ctrl Pts',(-8.91402577173804,4.50047177654324,2.60885089333748)) ;
#21677 = CARTESIAN_POINT('Ctrl Pts',(-9.00200639087887,4.51264465486516,2.65197256166106)) ;
#21678 = CARTESIAN_POINT('Ctrl Pts',(-9.16136120100629,4.56343058934306,2.75187845803316)) ;
#21679 = CARTESIAN_POINT('Ctrl Pts',(-9.23282794266408,4.60209590056535,2.80848839571465)) ;
#21680 = CARTESIAN_POINT('Ctrl Pts',(-9.32732933695259,4.67574116355534,2.89621445456693)) ;
#21681 = CARTESIAN_POINT('Ctrl Pts',(-9.36387082989461,4.711142531426,2.93411073778033)) ;
#21682 = CARTESIAN_POINT('Ctrl Pts',(-9.42828324602872,4.79043643796436,3.00844597489019)) ;
#21683 = CARTESIAN_POINT('Ctrl Pts',(-9.4562306030012,4.83434481308716,3.0448017613477)) ;
#21684 = CARTESIAN_POINT('Ctrl Pts',(-9.52791046153494,4.97144567551952,3.14552842549503)) ;
#21685 = CARTESIAN_POINT('Ctrl Pts',(-9.56444665447068,5.08718469591569,3.2110228981162)) ;
#21686 = CARTESIAN_POINT('Ctrl Pts',(-9.6097139388173,5.33803946527454,3.30043582906525)) ;
#21687 = CARTESIAN_POINT('Ctrl Pts',(-9.6192382673711,5.47323659419775,3.32372147829343)) ;
#21688 = CARTESIAN_POINT('Ctrl Pts',(-9.6192382673711,5.6,3.32372147829343)) ;
#21689 = CARTESIAN_POINT('Origin',(-8.68108404409997,5.6,2.97229330387474)) ;
#21690 = CARTESIAN_POINT('Origin',(-8.33803164073718,5.6,3.88808800801444)) ;
#21691 = CARTESIAN_POINT('Origin',(-8.33803164073718,5.6,3.88808800801444)) ;
#21692 = CARTESIAN_POINT('Origin',(-8.33803164073718,4.7,3.88808800801444)) ;
#21693 = CARTESIAN_POINT('Origin',(-9.12860070072158,5.6,1.14396208275687)) ;
#21694 = CARTESIAN_POINT('',(-10.1505515711168,5.6,0.737002111139838)) ;
#21695 = CARTESIAN_POINT('Origin',(-9.14983022680858,5.6,0.690184385194045)) ;
#21696 = CARTESIAN_POINT('',(-10.0185296933033,5.6,1.7905116850014)) ;
#21697 = CARTESIAN_POINT('Origin',(-9.12860070072158,5.6,1.14396208275687)) ;
#21698 = CARTESIAN_POINT('Origin',(-9.03720074846941,5.6,1.58894628507375)) ;
#21699 = CARTESIAN_POINT('Origin',(-8.84043936189492,5.6,2.54688670510862)) ;
#21700 = CARTESIAN_POINT('',(-8.84043936189492,5.6,1.14688670510861)) ;
#21701 = CARTESIAN_POINT('Origin',(-8.84043936189492,5.6,2.54688670510862)) ;
#21702 = CARTESIAN_POINT('Origin',(-9.19553212146245,5.6,-0.286686245139542)) ;
#21703 = CARTESIAN_POINT('',(-9.19553212146245,5.6,1.11331375486046)) ;
#21704 = CARTESIAN_POINT('Origin',(-9.19553212146245,5.6,-0.286686245139542)) ;
#21705 = CARTESIAN_POINT('Origin',(-9.12860070072158,5.6,1.14396208275687)) ;
#21706 = CARTESIAN_POINT('',(-9.99613400321582,5.6,0.467658919180464)) ;
#21707 = CARTESIAN_POINT('Origin',(-9.16206641109202,5.6,0.428637918808661)) ;
#21708 = CARTESIAN_POINT('',(-9.12860070072158,5.6,0.0439620827568656)) ;
#21709 = CARTESIAN_POINT('Origin',(-9.12860070072158,5.6,1.14396208275687)) ;
#21710 = CARTESIAN_POINT('Origin',(-9.19553212146245,5.6,-0.286686245139542)) ;
#21711 = CARTESIAN_POINT('',(-9.19553212146245,5.6,0.813313754860457)) ;
#21712 = CARTESIAN_POINT('Origin',(-9.19553212146245,5.6,-0.286686245139542)) ;
#21713 = CARTESIAN_POINT('Origin',(-9.03961155374625,5.6,-1.71038678589882)) ;
#21714 = CARTESIAN_POINT('',(-10.1419381783659,5.6,-0.847324787746512)) ;
#21715 = CARTESIAN_POINT('Origin',(-9.14607672781936,5.6,-0.738260220942957)) ;
#21716 = CARTESIAN_POINT('',(-9.03961155374625,5.6,-0.310386785898815)) ;
#21717 = CARTESIAN_POINT('Origin',(-9.03961155374625,5.6,-1.71038678589882)) ;
#21718 = CARTESIAN_POINT('Origin',(-9.19553212146245,5.6,-0.286686245139542)) ;
#21719 = CARTESIAN_POINT('',(-10.1750239396836,5.6,0.213909178369071)) ;
#21720 = CARTESIAN_POINT('Origin',(-9.19553212146245,5.6,-0.286686245139542)) ;
#21721 = CARTESIAN_POINT('Origin',(-9.17430259537545,5.6,0.167091452423278)) ;
#21722 = CARTESIAN_POINT('Origin',(-9.12860070072158,5.6,1.14396208275687)) ;
#21723 = CARTESIAN_POINT('',(-9.12860070072158,5.6,-0.256037917243135)) ;
#21724 = CARTESIAN_POINT('Origin',(-9.12860070072158,5.6,1.14396208275687)) ;
#21725 = CARTESIAN_POINT('Origin',(-9.03961155374625,5.6,-1.71038678589882)) ;
#21726 = CARTESIAN_POINT('',(-9.88753682467885,5.6,-2.41111693004411)) ;
#21727 = CARTESIAN_POINT('Origin',(-8.92066978252025,5.6,-2.14881322971911)) ;
#21728 = CARTESIAN_POINT('',(-10.0849283979359,5.6,-1.36787737689896)) ;
#21729 = CARTESIAN_POINT('Origin',(-9.03961155374625,5.6,-1.71038678589882)) ;
#21730 = CARTESIAN_POINT('Origin',(-9.08906694738934,5.6,-1.2588128100954)) ;
#21731 = CARTESIAN_POINT('Origin',(-9.19553212146245,5.6,-0.286686245139542)) ;
#21732 = CARTESIAN_POINT('',(-9.19553212146245,5.6,-1.68668624513954)) ;
#21733 = CARTESIAN_POINT('Origin',(-9.19553212146245,5.6,-0.286686245139542)) ;
#21734 = CARTESIAN_POINT('Origin',(-8.66461770315499,5.6,-3.0926364251514)) ;
#21735 = CARTESIAN_POINT('',(-8.66461770315499,5.6,-1.6926364251514)) ;
#21736 = CARTESIAN_POINT('Origin',(-8.66461770315499,5.6,-3.0926364251514)) ;
#21737 = CARTESIAN_POINT('Origin',(-9.03961155374625,5.6,-1.71038678589882)) ;
#21738 = CARTESIAN_POINT('',(-9.65796579805327,5.6,-2.62013292001948)) ;
#21739 = CARTESIAN_POINT('Origin',(-8.85211462845062,5.6,-2.40151160552511)) ;
#21740 = CARTESIAN_POINT('',(-9.03961155374625,5.6,-2.81038678589882)) ;
#21741 = CARTESIAN_POINT('Origin',(-9.03961155374625,5.6,-1.71038678589882)) ;
#21742 = CARTESIAN_POINT('Origin',(-8.66461770315499,5.6,-3.0926364251514)) ;
#21743 = CARTESIAN_POINT('',(-8.66461770315499,5.6,-1.9926364251514)) ;
#21744 = CARTESIAN_POINT('Origin',(-8.66461770315499,5.6,-3.0926364251514)) ;
#21745 = CARTESIAN_POINT('Origin',(-8.0796384750061,5.6,-4.39993660331612)) ;
#21746 = CARTESIAN_POINT('',(-9.3935128789311,5.6,-3.91647610781443)) ;
#21747 = CARTESIAN_POINT('Origin',(-8.47907208576222,5.6,-3.5072901547254)) ;
#21748 = CARTESIAN_POINT('',(-8.0796384750061,5.6,-2.99993660331612)) ;
#21749 = CARTESIAN_POINT('Origin',(-8.0796384750061,5.6,-4.39993660331612)) ;
#21750 = CARTESIAN_POINT('Origin',(-8.66461770315499,5.6,-3.0926364251514)) ;
#21751 = CARTESIAN_POINT('',(-9.75042651653959,5.6,-2.9165136816561)) ;
#21752 = CARTESIAN_POINT('Origin',(-8.66461770315499,5.6,-3.0926364251514)) ;
#21753 = CARTESIAN_POINT('Origin',(-8.78355947438099,5.6,-2.65420998133111)) ;
#21754 = CARTESIAN_POINT('Origin',(-9.03961155374625,5.6,-1.71038678589882)) ;
#21755 = CARTESIAN_POINT('',(-9.03961155374625,5.6,-3.11038678589882)) ;
#21756 = CARTESIAN_POINT('Origin',(-9.03961155374625,5.6,-1.71038678589882)) ;
#21757 = CARTESIAN_POINT('Origin',(-8.0796384750061,5.6,-4.39993660331612)) ;
#21758 = CARTESIAN_POINT('',(-8.67183891837006,5.6,-5.32692022500506)) ;
#21759 = CARTESIAN_POINT('Origin',(-7.83198567452591,5.6,-4.78076856363145)) ;
#21760 = CARTESIAN_POINT('',(-9.17962488556776,5.6,-4.39446882683115)) ;
#21761 = CARTESIAN_POINT('Origin',(-8.0796384750061,5.6,-4.39993660331612)) ;
#21762 = CARTESIAN_POINT('Origin',(-8.26518409239888,5.6,-3.98528287374212)) ;
#21763 = CARTESIAN_POINT('Origin',(-8.66461770315499,5.6,-3.0926364251514)) ;
#21764 = CARTESIAN_POINT('',(-8.66461770315499,5.6,-4.4926364251514)) ;
#21765 = CARTESIAN_POINT('Origin',(-8.66461770315499,5.6,-3.0926364251514)) ;
#21766 = CARTESIAN_POINT('Origin',(-7.29885073067936,5.6,-5.60060514688023)) ;
#21767 = CARTESIAN_POINT('',(-7.29885073067936,5.6,-4.20060514688023)) ;
#21768 = CARTESIAN_POINT('Origin',(-7.29885073067936,5.6,-5.60060514688023)) ;
#21769 = CARTESIAN_POINT('Origin',(-8.0796384750061,5.6,-4.39993660331612)) ;
#21770 = CARTESIAN_POINT('',(-8.38923404227527,5.6,-5.45546992099363)) ;
#21771 = CARTESIAN_POINT('Origin',(-7.68924460284273,5.6,-5.00027087509818)) ;
#21772 = CARTESIAN_POINT('',(-8.0796384750061,5.6,-5.49993660331612)) ;
#21773 = CARTESIAN_POINT('Origin',(-8.0796384750061,5.6,-4.39993660331612)) ;
#21774 = CARTESIAN_POINT('Origin',(-7.29885073067936,5.6,-5.60060514688023)) ;
#21775 = CARTESIAN_POINT('',(-7.29885073067936,5.6,-4.50060514688023)) ;
#21776 = CARTESIAN_POINT('Origin',(-7.29885073067936,5.6,-5.60060514688023)) ;
#21777 = CARTESIAN_POINT('Origin',(-6.34117671405231,5.6,-6.66554407990531)) ;
#21778 = CARTESIAN_POINT('',(-7.7400045754612,5.6,-6.60826743417404)) ;
#21779 = CARTESIAN_POINT('Origin',(-6.99509256607175,5.6,-5.9383859471302)) ;
#21780 = CARTESIAN_POINT('',(-6.34117671405231,5.6,-5.26554407990531)) ;
#21781 = CARTESIAN_POINT('Origin',(-6.34117671405231,5.6,-6.66554407990531)) ;
#21782 = CARTESIAN_POINT('Origin',(-7.29885073067936,5.6,-5.60060514688023)) ;
#21783 = CARTESIAN_POINT('',(-8.38635677500372,5.6,-5.76592484793852)) ;
#21784 = CARTESIAN_POINT('Origin',(-7.29885073067936,5.6,-5.60060514688023)) ;
#21785 = CARTESIAN_POINT('Origin',(-7.54650353115956,5.6,-5.21977318656491)) ;
#21786 = CARTESIAN_POINT('Origin',(-8.0796384750061,5.6,-4.39993660331612)) ;
#21787 = CARTESIAN_POINT('',(-8.0796384750061,5.6,-5.79993660331612)) ;
#21788 = CARTESIAN_POINT('Origin',(-8.0796384750061,5.6,-4.39993660331612)) ;
#21789 = CARTESIAN_POINT('Origin',(-6.34117671405231,5.6,-6.66554407990531)) ;
#21790 = CARTESIAN_POINT('',(-6.62059267994042,5.6,-7.7294645271225)) ;
#21791 = CARTESIAN_POINT('Origin',(-5.98867470720626,5.6,-6.95208766603628)) ;
#21792 = CARTESIAN_POINT('',(-7.38984688804938,5.6,-6.99764476669919)) ;
#21793 = CARTESIAN_POINT('Origin',(-6.34117671405231,5.6,-6.66554407990531)) ;
#21794 = CARTESIAN_POINT('Origin',(-6.64493487865992,5.6,-6.32776327965534)) ;
#21795 = CARTESIAN_POINT('Origin',(-7.29885073067936,5.6,-5.60060514688023)) ;
#21796 = CARTESIAN_POINT('',(-7.29885073067936,5.6,-7.00060514688023)) ;
#21797 = CARTESIAN_POINT('Origin',(-7.29885073067936,5.6,-5.60060514688023)) ;
#21798 = CARTESIAN_POINT('Origin',(-5.22982547448501,5.6,-7.56894480799191)) ;
#21799 = CARTESIAN_POINT('Origin',(-6.34117671405231,5.6,-6.66554407990531)) ;
#21800 = CARTESIAN_POINT('',(-5.78550109426866,4.76502012796642,-7.11724444394861)) ;
#21801 = CARTESIAN_POINT('Origin',(-5.78550109426866,5.6,-7.11724444394861)) ;
#21802 = CARTESIAN_POINT('Origin',(-5.22982547448501,5.6,-7.56894480799191)) ;
#21803 = CARTESIAN_POINT('Origin',(-3.99173039988154,5.6,-8.28891358470226)) ;
#21804 = CARTESIAN_POINT('',(-5.34073196819012,5.6,-8.66333950354468)) ;
#21805 = CARTESIAN_POINT('Origin',(-4.83712244512243,5.6,-7.79730685018094)) ;
#21806 = CARTESIAN_POINT('Origin',(-5.22982547448501,5.6,-7.56894480799191)) ;
#21807 = CARTESIAN_POINT('',(-6.21424545406522,5.6,-8.05977808294716)) ;
#21808 = CARTESIAN_POINT('Origin',(-5.22982547448501,5.6,-7.56894480799191)) ;
#21809 = CARTESIAN_POINT('Origin',(-5.58232748133106,5.6,-7.28240122186094)) ;
#21810 = CARTESIAN_POINT('Origin',(-6.34117671405231,5.6,-6.66554407990531)) ;
#21811 = CARTESIAN_POINT('Origin',(-3.99173039988154,5.6,-8.28891358470226)) ;
#21812 = CARTESIAN_POINT('',(-4.88804295231181,5.6,-8.92658419587697)) ;
#21813 = CARTESIAN_POINT('Origin',(-4.38443342924412,5.6,-8.06055154251323)) ;
#21814 = CARTESIAN_POINT('',(-3.99173039988154,5.6,-9.38891358470226)) ;
#21815 = CARTESIAN_POINT('Origin',(-3.99173039988154,5.6,-8.28891358470226)) ;
#21816 = CARTESIAN_POINT('',(-3.93143962342431,5.6,-9.38726007933598)) ;
#21817 = CARTESIAN_POINT('Origin',(-3.56834343193086,5.6,-8.453559771882)) ;
#21818 = CARTESIAN_POINT('Origin',(-5.22982547448501,5.6,-7.56894480799191)) ;
#21819 = CARTESIAN_POINT('Origin',(-2.6568964911086,5.6,-8.80800210238025)) ;
#21820 = CARTESIAN_POINT('Origin',(-3.99173039988154,5.6,-8.28891358470226)) ;
#21821 = CARTESIAN_POINT('',(-3.02168497866884,5.6,-7.77025003211321)) ;
#21822 = CARTESIAN_POINT('Origin',(-3.32431344549507,5.6,-8.54845784354125)) ;
#21823 = CARTESIAN_POINT('Origin',(-2.6568964911086,5.6,-8.80800210238025)) ;
#21824 = CARTESIAN_POINT('Origin',(-1.25767319645268,5.6,-9.11363034860009)) ;
#21825 = CARTESIAN_POINT('',(-2.42686958009725,5.6,-9.88368217573411)) ;
#21826 = CARTESIAN_POINT('Origin',(-2.21308628796886,5.6,-8.90494226522496)) ;
#21827 = CARTESIAN_POINT('Origin',(-2.6568964911086,5.6,-8.80800210238025)) ;
#21828 = CARTESIAN_POINT('',(-3.44337965055272,5.6,-9.57705622265449)) ;
#21829 = CARTESIAN_POINT('',(-2.71718726756582,5.6,-7.70965560774652)) ;
#21830 = CARTESIAN_POINT('Origin',(-3.08028345905927,5.6,-8.64335591520051)) ;
#21831 = CARTESIAN_POINT('',(-2.6568964911086,5.6,-9.90800210238025)) ;
#21832 = CARTESIAN_POINT('Origin',(-2.6568964911086,5.6,-8.80800210238025)) ;
#21833 = CARTESIAN_POINT('Origin',(-3.08028345905927,5.6,-8.64335591520051)) ;
#21834 = CARTESIAN_POINT('',(-2.6568964911086,5.6,-7.70800210238025)) ;
#21835 = CARTESIAN_POINT('Origin',(-2.6568964911086,5.6,-8.80800210238025)) ;
#21836 = CARTESIAN_POINT('Origin',(-3.99173039988154,5.6,-8.28891358470226)) ;
#21837 = CARTESIAN_POINT('Origin',(-1.25767319645268,5.6,-9.11363034860009)) ;
#21838 = CARTESIAN_POINT('',(-1.9152666917208,5.6,-9.99543009626452)) ;
#21839 = CARTESIAN_POINT('',(-1.48770010746402,5.6,-8.03795027524622)) ;
#21840 = CARTESIAN_POINT('Origin',(-1.70148339959241,5.6,-9.01669018575537)) ;
#21841 = CARTESIAN_POINT('',(-1.25767319645268,5.6,-10.2136303486001)) ;
#21842 = CARTESIAN_POINT('Origin',(-1.25767319645268,5.6,-9.11363034860009)) ;
#21843 = CARTESIAN_POINT('Origin',(-1.70148339959241,5.6,-9.01669018575537)) ;
#21844 = CARTESIAN_POINT('',(-1.25767319645268,5.6,-8.01363034860009)) ;
#21845 = CARTESIAN_POINT('Origin',(-1.25767319645268,5.6,-9.11363034860009)) ;
#21846 = CARTESIAN_POINT('',(-0.863484809736792,5.6,-10.1405750967625)) ;
#21847 = CARTESIAN_POINT('Origin',(-0.804195414779836,5.6,-9.14051516052749)) ;
#21848 = CARTESIAN_POINT('Origin',(-2.6568964911086,5.6,-8.80800210238025)) ;
#21849 = CARTESIAN_POINT('Origin',(0.172029571164298,5.6,-9.19839148039727)) ;
#21850 = CARTESIAN_POINT('Origin',(-1.25767319645268,5.6,-9.11363034860009)) ;
#21851 = CARTESIAN_POINT('',(-0.493406095500262,5.6,-8.32249458376462)) ;
#21852 = CARTESIAN_POINT('Origin',(-0.54282181264419,5.6,-9.15601091449868)) ;
#21853 = CARTESIAN_POINT('Origin',(0.172029571164298,5.6,-9.19839148039727)) ;
#21854 = CARTESIAN_POINT('Origin',(1.59756323453576,5.6,-9.06023132771231)) ;
#21855 = CARTESIAN_POINT('',(0.575602485190727,4.73397459621556,-8.65329616482006)) ;
#21856 = CARTESIAN_POINT('',(0.672767480349251,4.73397459621556,-9.65584262129112)) ;
#21857 = CARTESIAN_POINT('Origin',(0.624184982769988,5.6,-9.15456939305559)) ;
#21858 = CARTESIAN_POINT('Origin',(1.59756323453576,4.73397459621556,-9.06023132771231)) ;
#21859 = CARTESIAN_POINT('Origin',(1.59756323453576,4.7,-9.06023132771231)) ;
#21860 = CARTESIAN_POINT('Ctrl Pts',(0.575602485190727,4.73397459621556,-8.65329616482006)) ;
#21861 = CARTESIAN_POINT('Ctrl Pts',(0.553015540493783,4.68774565211319,-8.71002011751032)) ;
#21862 = CARTESIAN_POINT('Ctrl Pts',(0.532688177667106,4.64764400859375,-8.77533191459035)) ;
#21863 = CARTESIAN_POINT('Ctrl Pts',(0.498486784318542,4.57385160754098,-8.94720997429785)) ;
#21864 = CARTESIAN_POINT('Ctrl Pts',(0.492356730589572,4.55136544237033,-9.05969114282006)) ;
#21865 = CARTESIAN_POINT('Ctrl Pts',(0.513029963662795,4.55136544237033,-9.27299714389119)) ;
#21866 = CARTESIAN_POINT('Ctrl Pts',(0.540645980075106,4.57385160754098,-9.38220770413312)) ;
#21867 = CARTESIAN_POINT('Ctrl Pts',(0.607217027453607,4.64764400859375,-9.5443190805591)) ;
#21868 = CARTESIAN_POINT('Ctrl Pts',(0.639708063086502,4.68774565211319,-9.60451181368207)) ;
#21869 = CARTESIAN_POINT('Ctrl Pts',(0.672767480349251,4.73397459621556,-9.65584262129112)) ;
#21870 = CARTESIAN_POINT('Origin',(0.172029571164298,5.6,-9.19839148039727)) ;
#21871 = CARTESIAN_POINT('Origin',(1.59756323453576,5.6,-9.06023132771231)) ;
#21872 = CARTESIAN_POINT('',(0.965343734874546,5.6,-9.96039714812994)) ;
#21873 = CARTESIAN_POINT('Origin',(0.884796402850027,5.6,-9.12931140405479)) ;
#21874 = CARTESIAN_POINT('Origin',(0.172029571164298,5.6,-9.19839148039727)) ;
#21875 = CARTESIAN_POINT('Origin',(0.172029571164298,5.6,-9.19839148039727)) ;
#21876 = CARTESIAN_POINT('',(1.24204919246076,5.6,-10.1011971128789)) ;
#21877 = CARTESIAN_POINT('',(1.04876645339937,5.6,-8.10690971722908)) ;
#21878 = CARTESIAN_POINT('Origin',(1.14540782293007,5.6,-9.10405341505399)) ;
#21879 = CARTESIAN_POINT('Origin',(1.14540782293007,5.6,-9.10405341505399)) ;
#21880 = CARTESIAN_POINT('Origin',(1.59756323453576,5.6,-9.06023132771231)) ;
#21881 = CARTESIAN_POINT('',(1.59756323453576,5.6,-10.1602313277123)) ;
#21882 = CARTESIAN_POINT('Origin',(1.59756323453576,5.6,-9.06023132771231)) ;
#21883 = CARTESIAN_POINT('',(1.59756323453576,5.6,-7.96023132771231)) ;
#21884 = CARTESIAN_POINT('Origin',(1.59756323453576,5.6,-9.06023132771231)) ;
#21885 = CARTESIAN_POINT('Origin',(1.59756323453576,5.6,-9.06023132771231)) ;
#21886 = CARTESIAN_POINT('',(0.720826352300685,5.6,-10.1517130908805)) ;
#21887 = CARTESIAN_POINT('',(0.527543613239291,5.6,-8.15742569523067)) ;
#21888 = CARTESIAN_POINT('Origin',(0.624184982769988,5.6,-9.15456939305559)) ;
#21889 = CARTESIAN_POINT('Origin',(1.59756323453576,5.6,-9.06023132771231)) ;
#21890 = CARTESIAN_POINT('Origin',(0.172029571164298,5.6,-9.19839148039727)) ;
#21891 = CARTESIAN_POINT('',(-0.3407376054655,5.6,-10.1715666047049)) ;
#21892 = CARTESIAN_POINT('',(-0.222158815551588,5.6,-8.17144673223487)) ;
#21893 = CARTESIAN_POINT('Origin',(-0.281448210508544,5.6,-9.17150666846987)) ;
#21894 = CARTESIAN_POINT('',(0.172029571164298,5.6,-10.2983914803973)) ;
#21895 = CARTESIAN_POINT('Origin',(0.172029571164298,5.6,-9.19839148039727)) ;
#21896 = CARTESIAN_POINT('Origin',(-0.281448210508544,5.6,-9.17150666846987)) ;
#21897 = CARTESIAN_POINT('',(0.172029571164298,5.6,-8.09839148039727)) ;
#21898 = CARTESIAN_POINT('Origin',(0.172029571164298,5.6,-9.19839148039727)) ;
#21899 = CARTESIAN_POINT('Ctrl Pts',(0.720826352300685,5.6,-10.1517130908805)) ;
#21900 = CARTESIAN_POINT('Ctrl Pts',(0.720826352300685,5.46171298397554,-10.1517130908805)) ;
#21901 = CARTESIAN_POINT('Ctrl Pts',(0.696942796966399,5.31515492335585,-10.1336930651236)) ;
#21902 = CARTESIAN_POINT('Ctrl Pts',(0.610345858722663,5.04666004644025,-10.0546352509191)) ;
#21903 = CARTESIAN_POINT('Ctrl Pts',(0.548731949615678,4.9246088023834,-9.99278769580368)) ;
#21904 = CARTESIAN_POINT('Ctrl Pts',(0.4274343396663,4.72890627139334,-9.8353688728735)) ;
#21905 = CARTESIAN_POINT('Ctrl Pts',(0.359931166240814,4.64330837318027,-9.72855935219282)) ;
#21906 = CARTESIAN_POINT('Ctrl Pts',(0.280974043242848,4.55782771698258,-9.54105603524641)) ;
#21907 = CARTESIAN_POINT('Ctrl Pts',(0.258247910206437,4.53613333814489,-9.47410958337475)) ;
#21908 = CARTESIAN_POINT('Ctrl Pts',(0.223193451378181,4.50745592650039,-9.33621765108249)) ;
#21909 = CARTESIAN_POINT('Ctrl Pts',(0.210875366085843,4.50047177654324,-9.26526979989045)) ;
#21910 = CARTESIAN_POINT('Ctrl Pts',(0.197309571397666,4.50047177654324,-9.12529820444441)) ;
#21911 = CARTESIAN_POINT('Ctrl Pts',(0.195774098471602,4.50745592650039,-9.05330532190086)) ;
#21912 = CARTESIAN_POINT('Ctrl Pts',(0.203696395774903,4.53613333814489,-8.91124815988333)) ;
#21913 = CARTESIAN_POINT('Ctrl Pts',(0.213143660829931,4.55782771698258,-8.84118352027124)) ;
#21914 = CARTESIAN_POINT('Ctrl Pts',(0.254624526417109,4.64330837318027,-8.64200757059819)) ;
#21915 = CARTESIAN_POINT('Ctrl Pts',(0.300360457056649,4.72890627139334,-8.52422312010033)) ;
#21916 = CARTESIAN_POINT('Ctrl Pts',(0.389170995352308,4.9246088023834,-8.3464409942277)) ;
#21917 = CARTESIAN_POINT('Ctrl Pts',(0.437761432854958,5.04666004644025,-8.27391263251655)) ;
#21918 = CARTESIAN_POINT('Ctrl Pts',(0.507564998098324,5.31515492335585,-8.17969676347481)) ;
#21919 = CARTESIAN_POINT('Ctrl Pts',(0.527543613239291,5.46171298397554,-8.15742569523067)) ;
#21920 = CARTESIAN_POINT('Ctrl Pts',(0.527543613239291,5.6,-8.15742569523067)) ;
#21921 = CARTESIAN_POINT('Origin',(1.59756323453576,4.7,-9.06023132771231)) ;
#21922 = CARTESIAN_POINT('Origin',(-1.25767319645268,5.6,-9.11363034860009)) ;
#21923 = CARTESIAN_POINT('Origin',(-1.25767319645268,5.6,-9.11363034860009)) ;
#21924 = CARTESIAN_POINT('',(-1.25767319645267,7.,-9.11363034860001)) ;
#21925 = CARTESIAN_POINT('',(-1.34052789309705,5.6,-10.5111764477481)) ;
#21926 = CARTESIAN_POINT('Origin',(-1.25767319645268,5.6,-9.11363034860008)) ;
#21927 = CARTESIAN_POINT('',(-1.25767319645267,4.2,-9.11363034860001)) ;
#21928 = CARTESIAN_POINT('Origin',(-1.25767319645268,5.6,-9.11363034860008)) ;
#21929 = CARTESIAN_POINT('',(-1.55642729623381,5.6,-10.4813825146974)) ;
#21930 = CARTESIAN_POINT('Origin',(-1.25767319645268,5.6,-9.11363034860009)) ;
#21931 = CARTESIAN_POINT('Origin',(-1.25767319645268,5.6,-9.11363034860009)) ;
#21932 = CARTESIAN_POINT('Origin',(-2.6568964911086,5.6,-8.80800210238025)) ;
#21933 = CARTESIAN_POINT('',(-2.6568964911086,7.,-8.80800210238028)) ;
#21934 = CARTESIAN_POINT('',(-2.95565059088973,5.6,-10.1757542684776)) ;
#21935 = CARTESIAN_POINT('Origin',(-2.6568964911086,5.6,-8.80800210238025)) ;
#21936 = CARTESIAN_POINT('',(-2.6568964911086,4.2,-8.80800210238028)) ;
#21937 = CARTESIAN_POINT('Origin',(-2.6568964911086,5.6,-8.80800210238025)) ;
#21938 = CARTESIAN_POINT('',(-3.16430974470577,5.6,-10.1128131193762)) ;
#21939 = CARTESIAN_POINT('Origin',(-2.6568964911086,5.6,-8.80800210238025)) ;
#21940 = CARTESIAN_POINT('Origin',(-2.6568964911086,5.6,-8.80800210238025)) ;
#21941 = CARTESIAN_POINT('Origin',(-6.34117671405231,5.6,-6.66554407990531)) ;
#21942 = CARTESIAN_POINT('',(-6.34117671405228,7.,-6.66554407990528)) ;
#21943 = CARTESIAN_POINT('',(-7.22425828324403,5.6,-7.75189896766248)) ;
#21944 = CARTESIAN_POINT('Origin',(-6.34117671405231,5.6,-6.66554407990531)) ;
#21945 = CARTESIAN_POINT('',(-6.34117671405228,4.2,-6.66554407990528)) ;
#21946 = CARTESIAN_POINT('Origin',(-6.34117671405231,5.6,-6.66554407990531)) ;
#21947 = CARTESIAN_POINT('',(-7.38216319417279,5.6,-7.60167823065849)) ;
#21948 = CARTESIAN_POINT('Origin',(-6.34117671405231,5.6,-6.66554407990531)) ;
#21949 = CARTESIAN_POINT('Origin',(-6.34117671405231,5.6,-6.66554407990531)) ;
#21950 = CARTESIAN_POINT('Origin',(-7.29885073067936,5.6,-5.60060514688023)) ;
#21951 = CARTESIAN_POINT('',(-7.29885073067936,7.,-5.60060514688023)) ;
#21952 = CARTESIAN_POINT('',(-8.33983721079984,5.6,-6.53673929763341)) ;
#21953 = CARTESIAN_POINT('Origin',(-7.29885073067936,5.6,-5.60060514688023)) ;
#21954 = CARTESIAN_POINT('',(-7.29885073067936,4.2,-5.60060514688023)) ;
#21955 = CARTESIAN_POINT('Origin',(-7.29885073067936,5.6,-5.60060514688023)) ;
#21956 = CARTESIAN_POINT('',(-8.47251401051246,5.6,-6.36383152586056)) ;
#21957 = CARTESIAN_POINT('Origin',(-7.29885073067936,5.6,-5.60060514688023)) ;
#21958 = CARTESIAN_POINT('Origin',(-7.29885073067936,5.6,-5.60060514688023)) ;
#21959 = CARTESIAN_POINT('Origin',(-9.03961155374625,5.6,-1.71038678589882)) ;
#21960 = CARTESIAN_POINT('',(-9.03961155374629,7.,-1.71038678589883)) ;
#21961 = CARTESIAN_POINT('',(-10.3907718334498,5.6,-2.0769463288812)) ;
#21962 = CARTESIAN_POINT('Origin',(-9.03961155374625,5.6,-1.71038678589882)) ;
#21963 = CARTESIAN_POINT('',(-9.03961155374629,4.2,-1.71038678589883)) ;
#21964 = CARTESIAN_POINT('Origin',(-9.03961155374625,5.6,-1.71038678589882)) ;
#21965 = CARTESIAN_POINT('',(-10.4312904272575,5.6,-1.86280041069157)) ;
#21966 = CARTESIAN_POINT('Origin',(-9.03961155374625,5.6,-1.71038678589882)) ;
#21967 = CARTESIAN_POINT('Origin',(-9.03961155374625,5.6,-1.71038678589882)) ;
#21968 = CARTESIAN_POINT('Origin',(-9.19553212146245,5.6,-0.286686245139542)) ;
#21969 = CARTESIAN_POINT('',(-9.19553212146238,7.,-0.286686245139535)) ;
#21970 = CARTESIAN_POINT('',(-10.5872109949737,5.6,-0.439099869932289)) ;
#21971 = CARTESIAN_POINT('Origin',(-9.19553212146245,5.6,-0.286686245139542)) ;
#21972 = CARTESIAN_POINT('',(-9.19553212146238,4.2,-0.286686245139535)) ;
#21973 = CARTESIAN_POINT('Origin',(-9.19553212146245,5.6,-0.286686245139542)) ;
#21974 = CARTESIAN_POINT('',(-10.5940025134845,5.6,-0.221260236261659)) ;
#21975 = CARTESIAN_POINT('Origin',(-9.19553212146245,5.6,-0.286686245139543)) ;
#21976 = CARTESIAN_POINT('Origin',(-9.19553212146245,5.6,-0.286686245139543)) ;
#21977 = CARTESIAN_POINT('Origin',(-8.33803164073718,5.6,3.88808800801444)) ;
#21978 = CARTESIAN_POINT('',(-9.36813072379435,4.73397459621556,4.27395829591541)) ;
#21979 = CARTESIAN_POINT('',(-7.30793255768001,4.73397459621556,3.50221772011346)) ;
#21980 = CARTESIAN_POINT('Origin',(-8.33803164073718,5.6,3.88808800801444)) ;
#21981 = CARTESIAN_POINT('Origin',(-8.33803164073718,4.73397459621556,3.88808800801444)) ;
#21982 = CARTESIAN_POINT('Origin',(-8.33803164073718,5.6,3.88808800801444)) ;
#21983 = CARTESIAN_POINT('',(-7.02699644411896,5.6,3.39698036886774)) ;
#21984 = CARTESIAN_POINT('',(-7.07983245007737,5.9934418358376,3.41677248902982)) ;
#21985 = CARTESIAN_POINT('Origin',(-8.33803164073718,5.6,3.88808800801444)) ;
#21986 = CARTESIAN_POINT('',(-7.5297412638717,6.40829037686548,4.69637838487991)) ;
#21987 = CARTESIAN_POINT('Origin',(-8.33803164073718,5.6,3.88808800801444)) ;
#21988 = CARTESIAN_POINT('',(-9.64906683735539,5.6,4.37919564716113)) ;
#21989 = CARTESIAN_POINT('Origin',(-8.33803164073718,5.6,3.88808800801444)) ;
#21990 = CARTESIAN_POINT('Origin',(-8.33803164073718,5.6,3.88808800801444)) ;
#21991 = CARTESIAN_POINT('Origin',(-8.33803164073718,4.7,3.88808800801444)) ;
#21992 = CARTESIAN_POINT('',(-9.43803164073718,3.8,3.88808800801444)) ;
#21993 = CARTESIAN_POINT('Origin',(-8.33803164073718,3.8,3.88808800801444)) ;
#21994 = CARTESIAN_POINT('',(-9.43803164073718,4.65189880335233,3.88808800801446)) ;
#21995 = CARTESIAN_POINT('',(-9.43803164073718,4.7,3.88808800801444)) ;
#21996 = CARTESIAN_POINT('Ctrl Pts',(-9.43803164073718,4.65189880335233,3.88808800801448)) ;
#21997 = CARTESIAN_POINT('Ctrl Pts',(-9.43803164073718,4.67348663571234,3.94472968162414)) ;
#21998 = CARTESIAN_POINT('Ctrl Pts',(-9.43364416512203,4.6921524379,4.00185692423036)) ;
#21999 = CARTESIAN_POINT('Ctrl Pts',(-9.41328552009356,4.72400374275534,4.13153241586434)) ;
#22000 = CARTESIAN_POINT('Ctrl Pts',(-9.39435951087235,4.73397459621556,4.20393930153851)) ;
#22001 = CARTESIAN_POINT('Ctrl Pts',(-9.36813072379435,4.73397459621556,4.27395829591541)) ;
#22002 = CARTESIAN_POINT('Ctrl Pts',(-7.30793255768001,4.73397459621556,3.50221772011346)) ;
#22003 = CARTESIAN_POINT('Ctrl Pts',(-7.33416134475801,4.73397459621556,3.43219872573657)) ;
#22004 = CARTESIAN_POINT('Ctrl Pts',(-7.36746447425383,4.72400374275534,3.3651774419242)) ;
#22005 = CARTESIAN_POINT('Ctrl Pts',(-7.4459311319277,4.68822251881602,3.24032819717562)) ;
#22006 = CARTESIAN_POINT('Ctrl Pts',(-7.49109925396746,4.66259261868094,3.1824514714858)) ;
#22007 = CARTESIAN_POINT('Ctrl Pts',(-7.64041858377118,4.57386929426243,3.02541433890689)) ;
#22008 = CARTESIAN_POINT('Ctrl Pts',(-7.7594241100859,4.49983982293173,2.94283961099156)) ;
#22009 = CARTESIAN_POINT('Ctrl Pts',(-8.00214210356859,4.37384612030215,2.83240931234868)) ;
#22010 = CARTESIAN_POINT('Ctrl Pts',(-8.14325908220336,4.31153832429548,2.79560182561931)) ;
#22011 = CARTESIAN_POINT('Ctrl Pts',(-8.36279722995668,4.24614166874784,2.78592998438068)) ;
#22012 = CARTESIAN_POINT('Ctrl Pts',(-8.43733422265602,4.22885243350374,2.79007110227452)) ;
#22013 = CARTESIAN_POINT('Ctrl Pts',(-8.58385009380069,4.20577546283643,2.81334365875814)) ;
#22014 = CARTESIAN_POINT('Ctrl Pts',(-8.65582869467146,4.2,2.83248901060814)) ;
#22015 = CARTESIAN_POINT('Ctrl Pts',(-8.79197516260484,4.2,2.88348883930639)) ;
#22016 = CARTESIAN_POINT('Ctrl Pts',(-8.8588176742847,4.20577546283643,2.91634522549083)) ;
#22017 = CARTESIAN_POINT('Ctrl Pts',(-8.984564742228,4.22885243350374,2.99506108975102)) ;
#22018 = CARTESIAN_POINT('Ctrl Pts',(-9.04347823023389,4.24614166874784,3.04090989637728)) ;
#22019 = CARTESIAN_POINT('Ctrl Pts',(-9.20263169412595,4.31153832429548,3.19243784021295)) ;
#22020 = CARTESIAN_POINT('Ctrl Pts',(-9.28483603338533,4.37384612030215,3.31290044580185)) ;
#22021 = CARTESIAN_POINT('Ctrl Pts',(-9.39526633202821,4.49983982293173,3.55561843928454)) ;
#22022 = CARTESIAN_POINT('Ctrl Pts',(-9.43073199452746,4.57386929426243,3.69605735044247)) ;
#22023 = CARTESIAN_POINT('Ctrl Pts',(-9.43768488048529,4.63951461020542,3.85623687470378)) ;
#22024 = CARTESIAN_POINT('Ctrl Pts',(-9.43803164073718,4.64582185322758,3.87214344166024)) ;
#22025 = CARTESIAN_POINT('Ctrl Pts',(-9.43803164073718,4.65189880335233,3.88808800801448)) ;
#22026 = CARTESIAN_POINT('Origin',(1.59756323453576,4.7,-9.06023132771231)) ;
#22027 = CARTESIAN_POINT('',(0.197563234535756,3.8,-9.06023132771231)) ;
#22028 = CARTESIAN_POINT('Origin',(1.59756323453576,3.8,-9.06023132771231)) ;
#22029 = CARTESIAN_POINT('',(0.197563234535756,4.206529234206,-9.06023132771231)) ;
#22030 = CARTESIAN_POINT('',(0.197563234535756,4.7,-9.06023132771231)) ;
#22031 = CARTESIAN_POINT('',(1.73261590899087,5.6,-10.4537020935063)) ;
#22032 = CARTESIAN_POINT('Origin',(1.59756323453576,5.6,-9.06023132771231)) ;
#22033 = CARTESIAN_POINT('',(2.58751272819692,5.6,-10.0501808213735)) ;
#22034 = CARTESIAN_POINT('Origin',(1.59756323453576,5.6,-9.06023132771231)) ;
#22035 = CARTESIAN_POINT('',(1.46251056008064,5.6,-7.66676056191831)) ;
#22036 = CARTESIAN_POINT('Origin',(1.59756323453576,5.6,-9.06023132771231)) ;
#22037 = CARTESIAN_POINT('Origin',(1.59756323453576,5.6,-9.06023132771231)) ;
#22038 = CARTESIAN_POINT('Origin',(1.59756323453576,3.8,-9.06023132771231)) ;
#22039 = CARTESIAN_POINT('',(0.497563234535756,3.8,-9.06023132771231)) ;
#22040 = CARTESIAN_POINT('Origin',(1.59756323453576,3.8,-9.06023132771231)) ;
#22041 = CARTESIAN_POINT('Origin',(0.884796402850027,5.6,-9.12931140405479)) ;
#22042 = CARTESIAN_POINT('',(0.145771492360773,5.6,-7.7943765385289)) ;
#22043 = CARTESIAN_POINT('',(0.749743728394908,5.6,-7.73584063826079)) ;
#22044 = CARTESIAN_POINT('',(0.172029571164301,4.2,-9.1983914803973)) ;
#22045 = CARTESIAN_POINT('Origin',(0.172029571164302,5.6,-9.19839148039727)) ;
#22046 = CARTESIAN_POINT('',(0.172029571164301,7.,-9.1983914803973)) ;
#22047 = CARTESIAN_POINT('Origin',(0.172029571164298,5.6,-9.19839148039727)) ;
#22048 = CARTESIAN_POINT('Origin',(0.172029571164302,5.6,-9.19839148039727)) ;
#22049 = CARTESIAN_POINT('Origin',(1.59756323453576,5.6,-9.06023132771231)) ;
#22050 = CARTESIAN_POINT('Origin',(0.884796402850027,5.6,-9.12931140405479)) ;
#22051 = CARTESIAN_POINT('',(1.49145041889245,4.73397459621556,-7.96536144030274)) ;
#22052 = CARTESIAN_POINT('',(0.497563234535756,4.20402719569605,-9.06023132771226)) ;
#22053 = CARTESIAN_POINT('Ctrl Pts',(1.49145041889245,4.73397459621556,-7.96536144030274)) ;
#22054 = CARTESIAN_POINT('Ctrl Pts',(1.41702875426729,4.73397459621556,-7.97257425386995)) ;
#22055 = CARTESIAN_POINT('Ctrl Pts',(1.34367168114684,4.72400374275534,-7.98739622206835)) ;
#22056 = CARTESIAN_POINT('Ctrl Pts',(1.20276790583996,4.68822251881602,-8.03087583091053)) ;
#22057 = CARTESIAN_POINT('Ctrl Pts',(1.13517291153972,4.66259261868094,-8.05952528763701)) ;
#22058 = CARTESIAN_POINT('Ctrl Pts',(0.944840003140219,4.57386929426243,-8.16311248395889)) ;
#22059 = CARTESIAN_POINT('Ctrl Pts',(0.834278044165309,4.49983982293173,-8.25669108306875)) ;
#22060 = CARTESIAN_POINT('Ctrl Pts',(0.664790527398948,4.37384612030215,-8.4625571970336)) ;
#22061 = CARTESIAN_POINT('Ctrl Pts',(0.592713463708253,4.31153832429548,-8.58933925265689)) ;
#22062 = CARTESIAN_POINT('Ctrl Pts',(0.526550528703005,4.24614166874784,-8.79889356271373)) ;
#22063 = CARTESIAN_POINT('Ctrl Pts',(0.511258948151115,4.22885243350373,-8.87196256915488)) ;
#22064 = CARTESIAN_POINT('Ctrl Pts',(0.499550081017094,4.21135383689655,-8.98384305616054)) ;
#22065 = CARTESIAN_POINT('Ctrl Pts',(0.497563234535756,4.20690935315874,-9.02213729089606)) ;
#22066 = CARTESIAN_POINT('Ctrl Pts',(0.497563234535756,4.20402719569605,-9.0602313277122)) ;
#22067 = CARTESIAN_POINT('',(1.70367605017906,4.73397459621556,-10.1551012151219)) ;
#22068 = CARTESIAN_POINT('Ctrl Pts',(0.497563234535756,4.20402719569605,-9.0602313277122)) ;
#22069 = CARTESIAN_POINT('Ctrl Pts',(0.497563234535756,4.201329636592,-9.09588549205045)) ;
#22070 = CARTESIAN_POINT('Ctrl Pts',(0.499303157025686,4.2,-9.1313642304099)) ;
#22071 = CARTESIAN_POINT('Ctrl Pts',(0.509705723551869,4.2,-9.2386977016051)) ;
#22072 = CARTESIAN_POINT('Ctrl Pts',(0.524142440480705,4.20577546283643,-9.31176646842849)) ;
#22073 = CARTESIAN_POINT('Ctrl Pts',(0.567630390658757,4.22885243350374,-9.45360197375729)) ;
#22074 = CARTESIAN_POINT('Ctrl Pts',(0.596669004374252,4.24614166874784,-9.52237457768905)) ;
#22075 = CARTESIAN_POINT('Ctrl Pts',(0.701841811180312,4.31153832429548,-9.71532333653564)) ;
#22076 = CARTESIAN_POINT('Ctrl Pts',(0.796923704430307,4.37384612030215,-9.82590464740839)) ;
#22077 = CARTESIAN_POINT('Ctrl Pts',(1.00278981839516,4.49983982293173,-9.99539216417475)) ;
#22078 = CARTESIAN_POINT('Ctrl Pts',(1.12926420079653,4.57386929426243,-10.0659976284104)) ;
#22079 = CARTESIAN_POINT('Ctrl Pts',(1.33594685627334,4.66259261868093,-10.1311067920257)) ;
#22080 = CARTESIAN_POINT('Ctrl Pts',(1.40778543927975,4.68822251881602,-10.1462425978121)) ;
#22081 = CARTESIAN_POINT('Ctrl Pts',(1.55441629304583,4.72400374275534,-10.1618548687754)) ;
#22082 = CARTESIAN_POINT('Ctrl Pts',(1.62925438555391,4.73397459621556,-10.1623140286891)) ;
#22083 = CARTESIAN_POINT('Ctrl Pts',(1.70367605017906,4.73397459621556,-10.1551012151219)) ;
#22084 = CARTESIAN_POINT('Origin',(1.59756323453576,5.6,-9.06023132771231)) ;
#22085 = CARTESIAN_POINT('Origin',(-0.54282181264419,5.6,-9.15601091449868)) ;
#22086 = CARTESIAN_POINT('',(0.0891748745199313,5.6,-10.5959375795453)) ;
#22087 = CARTESIAN_POINT('Origin',(0.172029571164298,5.6,-9.19839148039727)) ;
#22088 = CARTESIAN_POINT('',(-0.625676509288564,5.6,-10.5535570136467)) ;
#22089 = CARTESIAN_POINT('Origin',(-1.25767319645268,5.6,-9.11363034860008)) ;
#22090 = CARTESIAN_POINT('Origin',(0.172029571164298,5.6,-9.19839148039727)) ;
#22091 = CARTESIAN_POINT('Origin',(-1.95728484378064,5.6,-8.96081622549017)) ;
#22092 = CARTESIAN_POINT('',(-2.25603894356177,5.6,-10.3285683915875)) ;
#22093 = CARTESIAN_POINT('Origin',(-2.65689649110859,5.6,-8.80800210238025)) ;
#22094 = CARTESIAN_POINT('Origin',(-3.32431344549507,5.6,-8.54845784354125)) ;
#22095 = CARTESIAN_POINT('',(-4.49914365347872,5.6,-9.59372460169817)) ;
#22096 = CARTESIAN_POINT('',(-3.83172669909225,5.6,-9.85326886053717)) ;
#22097 = CARTESIAN_POINT('',(-3.99173039988151,7.,-8.2889135847022)) ;
#22098 = CARTESIAN_POINT('Origin',(-3.99173039988154,5.6,-8.28891358470225)) ;
#22099 = CARTESIAN_POINT('',(-3.99173039988151,4.2,-8.2889135847022)) ;
#22100 = CARTESIAN_POINT('Origin',(-3.99173039988154,5.6,-8.28891358470225)) ;
#22101 = CARTESIAN_POINT('Origin',(-3.99173039988154,5.6,-8.28891358470225)) ;
#22102 = CARTESIAN_POINT('Origin',(-4.61077793718327,5.6,-7.92892919634708)) ;
#22103 = CARTESIAN_POINT('',(-4.69550574269427,5.6,-9.49916160343595)) ;
#22104 = CARTESIAN_POINT('Origin',(-3.99173039988154,5.6,-8.28891358470226)) ;
#22105 = CARTESIAN_POINT('',(-5.93360081729775,5.6,-8.7791928267256)) ;
#22106 = CARTESIAN_POINT('',(-5.31455327999601,5.6,-9.13917721508077)) ;
#22107 = CARTESIAN_POINT('',(-5.22982547448502,7.,-7.56894480799192)) ;
#22108 = CARTESIAN_POINT('Origin',(-5.22982547448501,5.6,-7.56894480799191)) ;
#22109 = CARTESIAN_POINT('',(-5.22982547448502,4.2,-7.56894480799192)) ;
#22110 = CARTESIAN_POINT('Origin',(-5.22982547448501,5.6,-7.56894480799191)) ;
#22111 = CARTESIAN_POINT('Origin',(-5.22982547448501,5.6,-7.56894480799191)) ;
#22112 = CARTESIAN_POINT('Origin',(-3.99173039988154,5.6,-8.28891358470226)) ;
#22113 = CARTESIAN_POINT('Origin',(-5.78550109426866,5.6,-7.11724444394861)) ;
#22114 = CARTESIAN_POINT('',(-6.11290704367673,5.6,-8.65529969574907)) ;
#22115 = CARTESIAN_POINT('Origin',(-5.22982547448501,5.6,-7.56894480799191)) ;
#22116 = CARTESIAN_POINT('',(-6.66858266346038,5.6,-8.20359933170578)) ;
#22117 = CARTESIAN_POINT('Origin',(-6.34117671405231,5.6,-6.66554407990531)) ;
#22118 = CARTESIAN_POINT('Origin',(-5.22982547448501,5.6,-7.56894480799191)) ;
#22119 = CARTESIAN_POINT('Origin',(-6.82001372236584,5.6,-6.13307461339277)) ;
#22120 = CARTESIAN_POINT('',(-7.86100020248631,5.6,-7.06920876414595)) ;
#22121 = CARTESIAN_POINT('Origin',(-7.29885073067936,5.6,-5.60060514688023)) ;
#22122 = CARTESIAN_POINT('Origin',(-7.68924460284273,5.6,-5.00027087509818)) ;
#22123 = CARTESIAN_POINT('',(-9.2533017548392,5.6,-5.16316298229645)) ;
#22124 = CARTESIAN_POINT('',(-8.86290788267583,5.6,-5.7634972540785)) ;
#22125 = CARTESIAN_POINT('',(-8.0796384750061,7.,-4.39993660331612)) ;
#22126 = CARTESIAN_POINT('Origin',(-8.0796384750061,5.6,-4.39993660331612)) ;
#22127 = CARTESIAN_POINT('',(-8.0796384750061,4.2,-4.39993660331612)) ;
#22128 = CARTESIAN_POINT('Origin',(-8.0796384750061,5.6,-4.39993660331613)) ;
#22129 = CARTESIAN_POINT('Origin',(-8.0796384750061,5.6,-4.39993660331612)) ;
#22130 = CARTESIAN_POINT('Origin',(-8.37212808908055,5.6,-3.74628651423376)) ;
#22131 = CARTESIAN_POINT('',(-9.35753504609195,5.6,-4.97175856302653)) ;
#22132 = CARTESIAN_POINT('Origin',(-8.0796384750061,5.6,-4.39993660331612)) ;
#22133 = CARTESIAN_POINT('',(-9.94251427424083,5.6,-3.6644583848618)) ;
#22134 = CARTESIAN_POINT('',(-9.65002466016639,5.6,-4.31810847394416)) ;
#22135 = CARTESIAN_POINT('',(-8.66461770315502,7.,-3.09263642515142)) ;
#22136 = CARTESIAN_POINT('Origin',(-8.66461770315499,5.6,-3.0926364251514)) ;
#22137 = CARTESIAN_POINT('',(-8.66461770315502,4.2,-3.09263642515142)) ;
#22138 = CARTESIAN_POINT('Origin',(-8.66461770315498,5.6,-3.09263642515141)) ;
#22139 = CARTESIAN_POINT('Origin',(-8.66461770315499,5.6,-3.0926364251514)) ;
#22140 = CARTESIAN_POINT('Origin',(-8.0796384750061,5.6,-4.39993660331612)) ;
#22141 = CARTESIAN_POINT('Origin',(-8.85211462845062,5.6,-2.40151160552511)) ;
#22142 = CARTESIAN_POINT('',(-10.0157779828585,5.6,-3.45919596813381)) ;
#22143 = CARTESIAN_POINT('Origin',(-8.66461770315498,5.6,-3.0926364251514)) ;
#22144 = CARTESIAN_POINT('',(-10.2032749081542,5.6,-2.7680711485075)) ;
#22145 = CARTESIAN_POINT('Origin',(-9.03961155374625,5.6,-1.71038678589882)) ;
#22146 = CARTESIAN_POINT('Origin',(-8.66461770315498,5.6,-3.0926364251514)) ;
#22147 = CARTESIAN_POINT('Origin',(-9.11757183760435,5.6,-0.998536515519179)) ;
#22148 = CARTESIAN_POINT('',(-10.5092507111156,5.6,-1.15095014031193)) ;
#22149 = CARTESIAN_POINT('Origin',(-9.19553212146245,5.6,-0.286686245139533)) ;
#22150 = CARTESIAN_POINT('Origin',(-9.16206641109202,5.6,0.428637918808661)) ;
#22151 = CARTESIAN_POINT('',(-10.5270710927436,5.6,1.20938809163475)) ;
#22152 = CARTESIAN_POINT('',(-10.5605368031141,5.6,0.494063927686545)) ;
#22153 = CARTESIAN_POINT('',(-9.12860070072155,7.,1.14396208275686)) ;
#22154 = CARTESIAN_POINT('Origin',(-9.12860070072158,5.6,1.14396208275687)) ;
#22155 = CARTESIAN_POINT('',(-9.12860070072155,4.2,1.14396208275686)) ;
#22156 = CARTESIAN_POINT('Origin',(-9.12860070072158,5.6,1.14396208275685)) ;
#22157 = CARTESIAN_POINT('Origin',(-9.12860070072158,5.6,1.14396208275687)) ;
#22158 = CARTESIAN_POINT('Origin',(-8.98452003130825,5.6,1.84542439393274)) ;
#22159 = CARTESIAN_POINT('',(-10.499970944786,5.6,1.42564213830696)) ;
#22160 = CARTESIAN_POINT('Origin',(-9.12860070072158,5.6,1.14396208275687)) ;
#22161 = CARTESIAN_POINT('',(-10.2118096059593,5.6,2.82856676065872)) ;
#22162 = CARTESIAN_POINT('',(-10.3558902753727,5.6,2.12710444948285)) ;
#22163 = CARTESIAN_POINT('',(-8.84043936189494,7.,2.54688670510862)) ;
#22164 = CARTESIAN_POINT('Origin',(-8.84043936189492,5.6,2.54688670510862)) ;
#22165 = CARTESIAN_POINT('',(-8.84043936189494,4.2,2.54688670510862)) ;
#22166 = CARTESIAN_POINT('Origin',(-8.84043936189492,5.6,2.54688670510861)) ;
#22167 = CARTESIAN_POINT('Origin',(-8.84043936189492,5.6,2.54688670510862)) ;
#22168 = CARTESIAN_POINT('Origin',(-9.12860070072158,5.6,1.14396208275687)) ;
#22169 = CARTESIAN_POINT('Origin',(-8.58923550131605,5.6,3.21748735656153)) ;
#22170 = CARTESIAN_POINT('',(-10.1514745585131,5.6,3.0379943442553)) ;
#22171 = CARTESIAN_POINT('Origin',(-8.84043936189492,5.6,2.54688670510862)) ;
#22172 = CARTESIAN_POINT('',(-9.90027069793426,5.6,3.70859499570822)) ;
#22173 = CARTESIAN_POINT('',(-9.73803164073718,5.10889236085331,3.88808800801444)) ;
#22174 = CARTESIAN_POINT('Origin',(-8.33803164073718,5.6,3.88808800801444)) ;
#22175 = CARTESIAN_POINT('Origin',(-8.33803164073718,5.6,3.88808800801444)) ;
#22176 = CARTESIAN_POINT('Origin',(-8.84043936189492,5.6,2.54688670510862)) ;
#22177 = CARTESIAN_POINT('Origin',(-8.58923550131605,5.6,3.21748735656153)) ;
#22178 = CARTESIAN_POINT('Origin',(-8.33803164073718,4.7,3.88808800801444)) ;
#22179 = CARTESIAN_POINT('',(-9.73803164073718,3.8,3.88808800801444)) ;
#22180 = CARTESIAN_POINT('',(-9.73803164073718,4.7,3.88808800801444)) ;
#22181 = CARTESIAN_POINT('Origin',(-8.33803164073718,3.8,3.88808800801444)) ;
#22182 = CARTESIAN_POINT('Origin',(-8.33803164073718,3.8,3.88808800801444)) ;
#22183 = CARTESIAN_POINT('Origin',(-8.84043936189492,5.6,2.54688670510862)) ;
#22184 = CARTESIAN_POINT('Origin',(-9.12860070072158,5.6,1.14396208275687)) ;
#22185 = CARTESIAN_POINT('Origin',(-8.66461770315499,5.6,-3.0926364251514)) ;
#22186 = CARTESIAN_POINT('Origin',(-8.0796384750061,5.6,-4.39993660331612)) ;
#22187 = CARTESIAN_POINT('Origin',(-5.22982547448501,5.6,-7.56894480799191)) ;
#22188 = CARTESIAN_POINT('Origin',(-3.99173039988154,5.6,-8.28891358470226)) ;
#22189 = CARTESIAN_POINT('Origin',(0.172029571164298,5.6,-9.19839148039727)) ;
#22190 = CARTESIAN_POINT('',(0.172029571164298,5.6,-10.5983914803973)) ;
#22191 = CARTESIAN_POINT('Origin',(0.172029571164298,5.6,-9.19839148039727)) ;
#22192 = CARTESIAN_POINT('Origin',(1.59756323453576,4.7,-9.06023132771231)) ;
#22193 = CARTESIAN_POINT('Origin',(1.59756323453576,4.73397459621556,-9.06023132771231)) ;
#22194 = CARTESIAN_POINT('',(0.497563234535756,4.7,-9.06023132771231)) ;
#22195 = CARTESIAN_POINT('Origin',(1.59756323453576,5.6,-9.06023132771231)) ;
#22196 = CARTESIAN_POINT('',(2.40585361140123,6.40829037686548,-8.25194095084684)) ;
#22197 = CARTESIAN_POINT('Origin',(1.59756323453576,5.6,-9.06023132771231)) ;
#22198 = CARTESIAN_POINT('Origin',(1.59756323453576,5.6,-9.06023132771231)) ;
#22199 = CARTESIAN_POINT('Origin',(-1.25767319645268,5.6,-9.11363034860009)) ;
#22200 = CARTESIAN_POINT('',(-1.77910365806296,5.6,-8.14506941933188)) ;
#22201 = CARTESIAN_POINT('Origin',(-1.95728484378064,5.6,-8.96081622549017)) ;
#22202 = CARTESIAN_POINT('Origin',(-2.6568964911086,5.6,-8.80800210238025)) ;
#22203 = CARTESIAN_POINT('Origin',(-3.99173039988154,5.6,-8.28891358470226)) ;
#22204 = CARTESIAN_POINT('',(-4.61077793718327,4.76502012796642,-7.92892919634708)) ;
#22205 = CARTESIAN_POINT('Origin',(-4.61077793718327,5.6,-7.92892919634708)) ;
#22206 = CARTESIAN_POINT('Origin',(-5.22982547448501,5.6,-7.56894480799191)) ;
#22207 = CARTESIAN_POINT('Origin',(-6.34117671405231,5.6,-6.66554407990531)) ;
#22208 = CARTESIAN_POINT('',(-7.44087283519418,5.6,-6.69139830868002)) ;
#22209 = CARTESIAN_POINT('Origin',(-6.82001372236584,5.6,-6.13307461339277)) ;
#22210 = CARTESIAN_POINT('',(-6.34117671405231,5.6,-5.56554407990531)) ;
#22211 = CARTESIAN_POINT('Origin',(-6.34117671405231,5.6,-6.66554407990531)) ;
#22212 = CARTESIAN_POINT('Origin',(-7.29885073067936,5.6,-5.60060514688023)) ;
#22213 = CARTESIAN_POINT('',(-7.29885073067936,5.6,-6.70060514688023)) ;
#22214 = CARTESIAN_POINT('Origin',(-7.29885073067936,5.6,-5.60060514688023)) ;
#22215 = CARTESIAN_POINT('Origin',(-8.0796384750061,5.6,-4.39993660331612)) ;
#22216 = CARTESIAN_POINT('',(-9.13428374293583,5.6,-4.08732924762303)) ;
#22217 = CARTESIAN_POINT('Origin',(-8.37212808908055,5.6,-3.74628651423376)) ;
#22218 = CARTESIAN_POINT('',(-8.0796384750061,5.6,-3.29993660331612)) ;
#22219 = CARTESIAN_POINT('Origin',(-8.0796384750061,5.6,-4.39993660331612)) ;
#22220 = CARTESIAN_POINT('Origin',(-8.66461770315499,5.6,-3.0926364251514)) ;
#22221 = CARTESIAN_POINT('',(-8.66461770315499,5.6,-4.1926364251514)) ;
#22222 = CARTESIAN_POINT('Origin',(-8.66461770315499,5.6,-3.0926364251514)) ;
#22223 = CARTESIAN_POINT('Origin',(-9.03961155374625,5.6,-1.71038678589882)) ;
#22224 = CARTESIAN_POINT('',(-9.94758887168739,5.6,-1.08943816475177)) ;
#22225 = CARTESIAN_POINT('Origin',(-9.11757183760435,5.6,-0.998536515519179)) ;
#22226 = CARTESIAN_POINT('',(-9.03961155374625,5.6,-0.610386785898816)) ;
#22227 = CARTESIAN_POINT('Origin',(-9.03961155374625,5.6,-1.71038678589882)) ;
#22228 = CARTESIAN_POINT('Origin',(-9.19553212146245,5.6,-0.286686245139542)) ;
#22229 = CARTESIAN_POINT('',(-9.19553212146245,5.6,-1.38668624513954)) ;
#22230 = CARTESIAN_POINT('Origin',(-9.19553212146245,5.6,-0.286686245139542)) ;
#22231 = CARTESIAN_POINT('Origin',(-9.12860070072158,5.6,1.14396208275687)) ;
#22232 = CARTESIAN_POINT('',(-9.80242471052222,5.6,2.01342237731677)) ;
#22233 = CARTESIAN_POINT('Origin',(-8.98452003130825,5.6,1.84542439393274)) ;
#22234 = CARTESIAN_POINT('',(-9.12860070072158,5.6,2.24396208275687)) ;
#22235 = CARTESIAN_POINT('Origin',(-9.12860070072158,5.6,1.14396208275687)) ;
#22236 = CARTESIAN_POINT('Origin',(-8.84043936189492,5.6,2.54688670510862)) ;
#22237 = CARTESIAN_POINT('',(-8.84043936189492,5.6,1.44688670510862)) ;
#22238 = CARTESIAN_POINT('Origin',(-8.84043936189492,5.6,2.54688670510862)) ;
#22239 = CARTESIAN_POINT('',(0.,0.,0.)) ;
#22240 = CARTESIAN_POINT('Origin',(2.5,-2.,13.2)) ;
#22241 = CARTESIAN_POINT('',(2.05,-2.,12.9)) ;
#22242 = CARTESIAN_POINT('',(2.95,-2.,12.9)) ;
#22243 = CARTESIAN_POINT('Origin',(2.5,-2.,12.9)) ;
#22244 = CARTESIAN_POINT('',(2.05,-2.,13.5)) ;
#22245 = CARTESIAN_POINT('',(2.05,-2.,13.2)) ;
#22246 = CARTESIAN_POINT('',(2.95,-2.,13.5)) ;
#22247 = CARTESIAN_POINT('Origin',(2.5,-2.,13.5)) ;
#22248 = CARTESIAN_POINT('',(2.95,-2.,13.2)) ;
#22249 = CARTESIAN_POINT('Origin',(2.95,-1.,13.2)) ;
#22250 = CARTESIAN_POINT('',(2.95,0.,12.9)) ;
#22251 = CARTESIAN_POINT('',(2.95,-1.05,12.9)) ;
#22252 = CARTESIAN_POINT('',(2.95,0.,13.5)) ;
#22253 = CARTESIAN_POINT('',(2.95,-2.95,13.5)) ;
#22254 = CARTESIAN_POINT('',(2.95,0.,13.2)) ;
#22255 = CARTESIAN_POINT('Origin',(2.5,0.,13.2)) ;
#22256 = CARTESIAN_POINT('',(2.05,0.,12.9)) ;
#22257 = CARTESIAN_POINT('Origin',(2.5,0.,12.9)) ;
#22258 = CARTESIAN_POINT('',(2.05,0.,13.5)) ;
#22259 = CARTESIAN_POINT('Origin',(2.5,0.,13.5)) ;
#22260 = CARTESIAN_POINT('',(2.05,0.,13.2)) ;
#22261 = CARTESIAN_POINT('Origin',(2.05,-1.,13.2)) ;
#22262 = CARTESIAN_POINT('',(2.05,-1.05,12.9)) ;
#22263 = CARTESIAN_POINT('',(2.05,-2.95,13.5)) ;
#22264 = CARTESIAN_POINT('Origin',(2.5,-4.9,11.5)) ;
#22265 = CARTESIAN_POINT('',(2.075,-5.2,11.5)) ;
#22266 = CARTESIAN_POINT('Origin',(2.5,-5.2,11.5)) ;
#22267 = CARTESIAN_POINT('',(2.075,-4.6,11.5)) ;
#22268 = CARTESIAN_POINT('',(2.075,-4.9,11.5)) ;
#22269 = CARTESIAN_POINT('Origin',(2.5,-4.6,11.5)) ;
#22270 = CARTESIAN_POINT('Origin',(-2.5,-2.,13.2)) ;
#22271 = CARTESIAN_POINT('',(-2.95,-2.,12.9)) ;
#22272 = CARTESIAN_POINT('',(-2.05,-2.,12.9)) ;
#22273 = CARTESIAN_POINT('Origin',(-2.5,-2.,12.9)) ;
#22274 = CARTESIAN_POINT('',(-2.95,-2.,13.5)) ;
#22275 = CARTESIAN_POINT('',(-2.95,-2.,13.2)) ;
#22276 = CARTESIAN_POINT('',(-2.05,-2.,13.5)) ;
#22277 = CARTESIAN_POINT('Origin',(-2.5,-2.,13.5)) ;
#22278 = CARTESIAN_POINT('',(-2.05,-2.,13.2)) ;
#22279 = CARTESIAN_POINT('Origin',(-2.05,-1.,13.2)) ;
#22280 = CARTESIAN_POINT('',(-2.05,0.,12.9)) ;
#22281 = CARTESIAN_POINT('',(-2.05,-1.05,12.9)) ;
#22282 = CARTESIAN_POINT('',(-2.05,0.,13.5)) ;
#22283 = CARTESIAN_POINT('',(-2.05,-2.95,13.5)) ;
#22284 = CARTESIAN_POINT('',(-2.05,0.,13.2)) ;
#22285 = CARTESIAN_POINT('Origin',(-2.5,0.,13.2)) ;
#22286 = CARTESIAN_POINT('',(-2.95,0.,12.9)) ;
#22287 = CARTESIAN_POINT('Origin',(-2.5,0.,12.9)) ;
#22288 = CARTESIAN_POINT('',(-2.95,0.,13.5)) ;
#22289 = CARTESIAN_POINT('Origin',(-2.5,0.,13.5)) ;
#22290 = CARTESIAN_POINT('',(-2.95,0.,13.2)) ;
#22291 = CARTESIAN_POINT('Origin',(-2.95,-1.,13.2)) ;
#22292 = CARTESIAN_POINT('',(-2.95,-1.05,12.9)) ;
#22293 = CARTESIAN_POINT('',(-2.95,-2.95,13.5)) ;
#22294 = CARTESIAN_POINT('Origin',(-2.5,-4.9,11.5)) ;
#22295 = CARTESIAN_POINT('',(-2.925,-5.2,11.5)) ;
#22296 = CARTESIAN_POINT('Origin',(-2.5,-5.2,11.5)) ;
#22297 = CARTESIAN_POINT('',(-2.925,-4.6,11.5)) ;
#22298 = CARTESIAN_POINT('',(-2.925,-4.9,11.5)) ;
#22299 = CARTESIAN_POINT('Origin',(-2.5,-4.6,11.5)) ;
#22300 = CARTESIAN_POINT('Origin',(0.,-1.1,12.9)) ;
#22301 = CARTESIAN_POINT('',(-4.5,-4.6,12.9)) ;
#22302 = CARTESIAN_POINT('',(4.5,-4.6,12.9)) ;
#22303 = CARTESIAN_POINT('',(0.,-4.6,12.9)) ;
#22304 = CARTESIAN_POINT('',(-4.5,3.,12.9)) ;
#22305 = CARTESIAN_POINT('',(-4.5,-1.1,12.9)) ;
#22306 = CARTESIAN_POINT('',(4.5,3.,12.9)) ;
#22307 = CARTESIAN_POINT('',(0.,3.,12.9)) ;
#22308 = CARTESIAN_POINT('',(4.5,-1.1,12.9)) ;
#22309 = CARTESIAN_POINT('Origin',(0.,3.,13.2)) ;
#22310 = CARTESIAN_POINT('',(4.5,3.,13.5)) ;
#22311 = CARTESIAN_POINT('',(4.5,3.,13.2)) ;
#22312 = CARTESIAN_POINT('',(-4.5,3.,13.5)) ;
#22313 = CARTESIAN_POINT('',(-4.5,3.,13.2)) ;
#22314 = CARTESIAN_POINT('',(0.,3.,13.5)) ;
#22315 = CARTESIAN_POINT('Origin',(0.,-4.6,11.5)) ;
#22316 = CARTESIAN_POINT('',(4.5,-4.6,9.5)) ;
#22317 = CARTESIAN_POINT('',(4.5,-4.6,11.5)) ;
#22318 = CARTESIAN_POINT('',(-4.5,-4.6,9.5)) ;
#22319 = CARTESIAN_POINT('',(0.,-4.6,9.5)) ;
#22320 = CARTESIAN_POINT('',(-4.5,-4.6,11.5)) ;
#22321 = CARTESIAN_POINT('Origin',(4.5,-4.9,11.5)) ;
#22322 = CARTESIAN_POINT('',(4.5,-5.2,13.5)) ;
#22323 = CARTESIAN_POINT('',(4.5,-5.2,9.5)) ;
#22324 = CARTESIAN_POINT('',(4.5,-5.2,11.5)) ;
#22325 = CARTESIAN_POINT('',(4.5,-4.9,9.5)) ;
#22326 = CARTESIAN_POINT('',(4.5,-4.9,13.5)) ;
#22327 = CARTESIAN_POINT('Origin',(0.,-4.9,13.5)) ;
#22328 = CARTESIAN_POINT('',(-4.5,-5.2,13.5)) ;
#22329 = CARTESIAN_POINT('',(-4.5,-4.9,13.5)) ;
#22330 = CARTESIAN_POINT('',(0.,-5.2,13.5)) ;
#22331 = CARTESIAN_POINT('Origin',(0.,-4.9,9.5)) ;
#22332 = CARTESIAN_POINT('',(-4.5,-5.2,9.5)) ;
#22333 = CARTESIAN_POINT('',(0.,-5.2,9.5)) ;
#22334 = CARTESIAN_POINT('',(-4.5,-4.9,9.5)) ;
#22335 = CARTESIAN_POINT('Origin',(0.,-5.2,11.5)) ;
#22336 = CARTESIAN_POINT('',(-4.5,-5.2,11.5)) ;
#22337 = CARTESIAN_POINT('Origin',(-4.5,-4.9,11.5)) ;
#22338 = CARTESIAN_POINT('',(0.,0.,0.)) ;
#22339 = CARTESIAN_POINT('',(0.,0.,0.)) ;
#22340 = CARTESIAN_POINT('',(0.,0.,0.)) ;
#22341 = CARTESIAN_POINT('',(0.,0.,0.)) ;
#22342 = CARTESIAN_POINT('',(0.,0.,0.)) ;
#22343 = CARTESIAN_POINT('',(0.,0.,0.)) ;
#22344 = CARTESIAN_POINT('',(0.,0.,0.)) ;
#22345 = CARTESIAN_POINT('',(0.,0.,0.)) ;
#22346 = CARTESIAN_POINT('',(0.,0.,0.)) ;
#22347 = CARTESIAN_POINT('',(0.,0.,0.)) ;
#22348 = CARTESIAN_POINT('',(0.,0.,0.)) ;
#22349 = CARTESIAN_POINT('',(0.,0.,0.)) ;
#22350 = CARTESIAN_POINT('',(0.,0.,0.)) ;
#22351 = CARTESIAN_POINT('',(-3.48860546192182,0.,9.58486473201627)) ;
#22352 = CARTESIAN_POINT('',(9.58486473201627,0.,3.48860546192182)) ;
#22353 = CARTESIAN_POINT('',(-9.58486473201627,0.,-3.48860546192182)) ;
#22354 = CARTESIAN_POINT('',(3.48860546192182,0.,-9.58486473201627)) ;
#22355 = CARTESIAN_POINT('',(0.,0.,0.)) ;
#22356 = CARTESIAN_POINT('',(0.,0.,0.)) ;
#22357 = CARTESIAN_POINT('',(0.,0.,0.)) ;
#22358 = CARTESIAN_POINT('',(0.,0.,0.)) ;
#22359 = CARTESIAN_POINT('',(0.,0.,0.)) ;
#22360 = CARTESIAN_POINT('',(0.,0.,0.)) ;
#22361 = CARTESIAN_POINT('',(0.,0.,0.)) ;
#22362 = CARTESIAN_POINT('Ctrl Pts',(-29.7879704997762,4.1982235964065,15.004760387006)) ;
#22363 = CARTESIAN_POINT('Ctrl Pts',(-28.9765416158345,3.49667700708559,12.8596184051575)) ;
#22364 = CARTESIAN_POINT('Ctrl Pts',(-27.6245525523466,2.32566824542574,9.28480711044218)) ;
#22365 = CARTESIAN_POINT('Ctrl Pts',(-26.005233549839,0.90734538201738,4.99813706529367)) ;
#22366 = CARTESIAN_POINT('Ctrl Pts',(-24.9352460971343,-0.0565633455803164,
2.14271187262585)) ;
#22367 = CARTESIAN_POINT('Ctrl Pts',(-24.4110437339872,-0.552959968693851,
0.715613732723115)) ;
#22368 = CARTESIAN_POINT('Ctrl Pts',(-24.1589049321087,-0.806397566452131,
-5.70268832156273E-10)) ;
#22369 = CARTESIAN_POINT('Ctrl Pts',(-29.7880085856475,3.05586778828661,15.0030622151785)) ;
#22370 = CARTESIAN_POINT('Ctrl Pts',(-28.9985961339778,2.49325092521034,12.8575620409374)) ;
#22371 = CARTESIAN_POINT('Ctrl Pts',(-27.6830843893262,1.55403581881225,9.28200460526821)) ;
#22372 = CARTESIAN_POINT('Ctrl Pts',(-26.1062403134519,0.416417293310764,
4.99328651815293)) ;
#22373 = CARTESIAN_POINT('Ctrl Pts',(-25.0612351613324,-0.357449889914694,
2.13576141937932)) ;
#22374 = CARTESIAN_POINT('Ctrl Pts',(-24.5450981755029,-0.75720095086868,
0.707828841054705)) ;
#22375 = CARTESIAN_POINT('Ctrl Pts',(-24.2953334946171,-0.964113147540073,
-0.00706604193771441)) ;
#22376 = CARTESIAN_POINT('Ctrl Pts',(-29.7880984019284,0.77088432617787,15.0004371510981)) ;
#22377 = CARTESIAN_POINT('Ctrl Pts',(-29.0320656779143,0.477248554069186,
12.854352481685)) ;
#22378 = CARTESIAN_POINT('Ctrl Pts',(-27.7718140786327,-0.0129653268429286,
9.2776079223855)) ;
#22379 = CARTESIAN_POINT('Ctrl Pts',(-26.2598801085757,-0.606556867865899,
4.9857552974963)) ;
#22380 = CARTESIAN_POINT('Ctrl Pts',(-25.252746996273,-1.01128931246026,2.12475519883151)) ;
#22381 = CARTESIAN_POINT('Ctrl Pts',(-24.7498599068977,-1.22062620685322,
0.694492730733407)) ;
#22382 = CARTESIAN_POINT('Ctrl Pts',(-24.5000082407848,-1.33280874531094,
-0.0206610680077742)) ;
#22383 = CARTESIAN_POINT('Ctrl Pts',(-29.7881434031396,-3.22828201380981,
14.9994444092913)) ;
#22384 = CARTESIAN_POINT('Ctrl Pts',(-29.0444129979685,-3.06557811875762,
12.8531317839584)) ;
#22385 = CARTESIAN_POINT('Ctrl Pts',(-27.8048257006081,-2.79391277080305,
9.27588292843548)) ;
#22386 = CARTESIAN_POINT('Ctrl Pts',(-26.317044506741,-2.46505212911362,4.98280140110366)) ;
#22387 = CARTESIAN_POINT('Ctrl Pts',(-25.3239448603091,-2.24067401478496,
2.12040334815057)) ;
#22388 = CARTESIAN_POINT('Ctrl Pts',(-24.8262703953289,-2.12469662243215,
0.688894444476874)) ;
#22389 = CARTESIAN_POINT('Ctrl Pts',(-24.5752760211477,-2.06194576114233,
-0.0267624859759424)) ;
#22390 = CARTESIAN_POINT('Ctrl Pts',(-29.7880276285832,-6.08468988422692,
15.0022131292648)) ;
#22391 = CARTESIAN_POINT('Ctrl Pts',(-29.0097274305354,-5.59160872404636,
12.8565299181811)) ;
#22392 = CARTESIAN_POINT('Ctrl Pts',(-27.7122818351144,-4.76817410676846,
9.28063964648335)) ;
#22393 = CARTESIAN_POINT('Ctrl Pts',(-26.1568276984181,-3.77112949936236,
4.99094264430357)) ;
#22394 = CARTESIAN_POINT('Ctrl Pts',(-25.1243483646472,-3.09226178271257,
2.13236773367943)) ;
#22395 = CARTESIAN_POINT('Ctrl Pts',(-24.6123236175051,-2.74112531762835,
0.704011231405586)) ;
#22396 = CARTESIAN_POINT('Ctrl Pts',(-24.3635477758713,-2.557029061916,-0.0105990626214356)) ;
#22397 = CARTESIAN_POINT('Ctrl Pts',(-29.7879704997762,-7.79822359640676,
15.004760387006)) ;
#22398 = CARTESIAN_POINT('Ctrl Pts',(-28.9765416158345,-7.09667700708582,
12.8596184051575)) ;
#22399 = CARTESIAN_POINT('Ctrl Pts',(-27.6245525523466,-5.92566824542591,
9.28480711044218)) ;
#22400 = CARTESIAN_POINT('Ctrl Pts',(-26.0052335498389,-4.50734538201749,
4.99813706529367)) ;
#22401 = CARTESIAN_POINT('Ctrl Pts',(-24.9352460971343,-3.54343665441975,
2.14271187262586)) ;
#22402 = CARTESIAN_POINT('Ctrl Pts',(-24.4110437339872,-3.0470400313062,0.715613732723117)) ;
#22403 = CARTESIAN_POINT('Ctrl Pts',(-24.1589049321087,-2.79360243354791,
-5.70267222332888E-10)) ;
#22404 = CARTESIAN_POINT('',(-29.7862997944388,-7.58988663107372,15.)) ;
#22405 = CARTESIAN_POINT('',(-29.7862997944388,3.98988663107372,15.)) ;
#22406 = CARTESIAN_POINT('Ctrl Pts',(-29.7862997944388,-7.58988663107372,
15.)) ;
#22407 = CARTESIAN_POINT('Ctrl Pts',(-29.7874854452745,-5.67140621570733,
15.)) ;
#22408 = CARTESIAN_POINT('Ctrl Pts',(-29.7880884026998,-3.78346330304678,
15.)) ;
#22409 = CARTESIAN_POINT('Ctrl Pts',(-29.7881190038692,0.0862220953979725,
15.)) ;
#22410 = CARTESIAN_POINT('Ctrl Pts',(-29.7875160987196,2.02180642423597,15.)) ;
#22411 = CARTESIAN_POINT('Ctrl Pts',(-29.7862997944388,3.98988663107372,15.)) ;
#22412 = CARTESIAN_POINT('',(-24.1927688881933,-2.82237333273713,0.0891518022986763)) ;
#22413 = CARTESIAN_POINT('Ctrl Pts',(-24.1927688881933,-2.82237333273713,
0.0891518022986763)) ;
#22414 = CARTESIAN_POINT('Ctrl Pts',(-24.1934570101164,-2.82295781734209,
0.0909648418835227)) ;
#22415 = CARTESIAN_POINT('Ctrl Pts',(-24.1941451106354,-2.82354227530196,
0.092777911525871)) ;
#22416 = CARTESIAN_POINT('Ctrl Pts',(-24.1948331817638,-2.82412669991032,
0.094590989728832)) ;
#22417 = CARTESIAN_POINT('Ctrl Pts',(-24.6678538621346,-3.22589464870741,
1.34100789310195)) ;
#22418 = CARTESIAN_POINT('Ctrl Pts',(-25.0587313958119,-3.55537106707809,
2.39676629444992)) ;
#22419 = CARTESIAN_POINT('Ctrl Pts',(-26.0013963074572,-4.35779250443395,
4.91745743939535)) ;
#22420 = CARTESIAN_POINT('Ctrl Pts',(-26.2448135648579,-4.56499574616668,
5.56835652100608)) ;
#22421 = CARTESIAN_POINT('Ctrl Pts',(-26.5249696032859,-4.803694805458,6.31696827513027)) ;
#22422 = CARTESIAN_POINT('Ctrl Pts',(-26.852785444491,-5.0833030095669,7.19178833495937)) ;
#22423 = CARTESIAN_POINT('Ctrl Pts',(-26.9542070569034,-5.16980985682658,
7.46244536212537)) ;
#22424 = CARTESIAN_POINT('Ctrl Pts',(-27.0601952624917,-5.26023714996938,
7.74519169930263)) ;
#22425 = CARTESIAN_POINT('Ctrl Pts',(-27.1656849213349,-5.35026234294172,
8.02651094121919)) ;
#22426 = CARTESIAN_POINT('Ctrl Pts',(-28.0317195564602,-6.0893389121793,10.3360473422142)) ;
#22427 = CARTESIAN_POINT('Ctrl Pts',(-28.9467094713777,-6.87166395755108,
12.769529848754)) ;
#22428 = CARTESIAN_POINT('Ctrl Pts',(-29.7862997944388,-7.58988663107372,
15.)) ;
#22429 = CARTESIAN_POINT('',(-24.1589049319639,-2.79360243342489,-4.75519821435677E-10)) ;
#22430 = CARTESIAN_POINT('Ctrl Pts',(-24.1589049321088,-2.79360243354777,
-5.70273040595426E-10)) ;
#22431 = CARTESIAN_POINT('Ctrl Pts',(-24.1695174648536,-2.80262121435912,
0.0279159200689838)) ;
#22432 = CARTESIAN_POINT('Ctrl Pts',(-24.1801188171535,-2.81162839675808,
0.0558294517448662)) ;
#22433 = CARTESIAN_POINT('Ctrl Pts',(-24.1907006565412,-2.82061729735981,
0.083715933657329)) ;
#22434 = CARTESIAN_POINT('Ctrl Pts',(-24.1913885763442,-2.82120166105167,
0.0855288191530417)) ;
#22435 = CARTESIAN_POINT('Ctrl Pts',(-24.1920764667909,-2.82178599256751,
0.0873417302858431)) ;
#22436 = CARTESIAN_POINT('Ctrl Pts',(-24.1927643256631,-2.8223702901168,0.0891546605139208)) ;
#22437 = CARTESIAN_POINT('',(-24.1589049319644,-0.806397566574673,-4.7482698675716E-10)) ;
#22438 = CARTESIAN_POINT('Ctrl Pts',(-24.1589049323255,-0.8063975662679,1.09620886621735E-16)) ;
#22439 = CARTESIAN_POINT('Ctrl Pts',(-24.283597624207,-0.945716532508702,
1.09623628239148E-16)) ;
#22440 = CARTESIAN_POINT('Ctrl Pts',(-24.3808054594196,-1.10713716355173,
-1.18390020009684E-12)) ;
#22441 = CARTESIAN_POINT('Ctrl Pts',(-24.512802414918,-1.46434976621459,-1.18390020009684E-12)) ;
#22442 = CARTESIAN_POINT('Ctrl Pts',(-24.5438655539448,-1.6575893537085,-1.38777878078145E-15)) ;
#22443 = CARTESIAN_POINT('Ctrl Pts',(-24.5311976151215,-2.02703780425878,
-1.38777878078145E-15)) ;
#22444 = CARTESIAN_POINT('Ctrl Pts',(-24.4941869311108,-2.20048822446343,
1.4585554986013E-14)) ;
#22445 = CARTESIAN_POINT('Ctrl Pts',(-24.3634307218009,-2.52123101046768,
1.4585554986013E-14)) ;
#22446 = CARTESIAN_POINT('Ctrl Pts',(-24.2725344551939,-2.66664433040153,
3.20484281317344E-16)) ;
#22447 = CARTESIAN_POINT('Ctrl Pts',(-24.1589049323255,-2.79360243373209,
3.20484666411866E-16)) ;
#22448 = CARTESIAN_POINT('',(-24.1927688881933,-0.777626667262871,0.0891518022986696)) ;
#22449 = CARTESIAN_POINT('Ctrl Pts',(-24.1927640983708,-0.777630284368101,
0.0891545456106432)) ;
#22450 = CARTESIAN_POINT('Ctrl Pts',(-24.1920762479986,-0.778214559997417,
0.0873416191464197)) ;
#22451 = CARTESIAN_POINT('Ctrl Pts',(-24.1913883666309,-0.778798869477654,
0.0855287137798584)) ;
#22452 = CARTESIAN_POINT('Ctrl Pts',(-24.1907004548719,-0.779383212398548,
0.0837158318083245)) ;
#22453 = CARTESIAN_POINT('Ctrl Pts',(-24.1801187424362,-0.788371790761656,
0.0558294125816257)) ;
#22454 = CARTESIAN_POINT('Ctrl Pts',(-24.1695174641247,-0.797378786260146,
0.0279159181518874)) ;
#22455 = CARTESIAN_POINT('Ctrl Pts',(-24.158904932109,-0.806397566451893,
-5.69441659411157E-10)) ;
#22456 = CARTESIAN_POINT('Ctrl Pts',(-29.7862997944388,3.98988663107372,15.)) ;
#22457 = CARTESIAN_POINT('Ctrl Pts',(-29.1328907328544,3.43093163811475,13.2641422031832)) ;
#22458 = CARTESIAN_POINT('Ctrl Pts',(-28.4338012516642,2.8331537658536,11.4053304313931)) ;
#22459 = CARTESIAN_POINT('Ctrl Pts',(-27.7476813820024,2.24714826965254,9.5776689963089)) ;
#22460 = CARTESIAN_POINT('Ctrl Pts',(-27.5821910090633,2.10580522975702,9.13684169211246)) ;
#22461 = CARTESIAN_POINT('Ctrl Pts',(-27.4174547163538,1.96514782273,8.69782652065271)) ;
#22462 = CARTESIAN_POINT('Ctrl Pts',(-27.2542924969021,1.82588555176052,8.26278713091792)) ;
#22463 = CARTESIAN_POINT('Ctrl Pts',(-27.144362859745,1.73205837186077,7.96968176361375)) ;
#22464 = CARTESIAN_POINT('Ctrl Pts',(-27.0345809892665,1.63838104542639,7.67686898630538)) ;
#22465 = CARTESIAN_POINT('Ctrl Pts',(-26.926973332117,1.54658537416295,7.38975189096568)) ;
#22466 = CARTESIAN_POINT('Ctrl Pts',(-25.4222119002236,0.262935219600215,
3.37477058806011)) ;
#22467 = CARTESIAN_POINT('Ctrl Pts',(-24.8950276354157,-0.182007944164745,
1.94978881746105)) ;
#22468 = CARTESIAN_POINT('Ctrl Pts',(-24.3591765397677,-0.636412221527215,
0.52907137988932)) ;
#22469 = CARTESIAN_POINT('Ctrl Pts',(-24.304864353331,-0.682469213908392,
0.385071916288646)) ;
#22470 = CARTESIAN_POINT('Ctrl Pts',(-24.2504445757749,-0.728638841618619,
0.241127884134561)) ;
#22471 = CARTESIAN_POINT('Ctrl Pts',(-24.1948331817649,-0.775873300087209,
0.0945909897337519)) ;
#22472 = CARTESIAN_POINT('Ctrl Pts',(-24.1941451093438,-0.776457725793072,
0.0927779081250757)) ;
#22473 = CARTESIAN_POINT('Ctrl Pts',(-24.1934570114089,-0.777042181560007,
0.0909648452891593)) ;
#22474 = CARTESIAN_POINT('Ctrl Pts',(-24.1927688881933,-0.777626667262871,
0.0891518022986696)) ;
#22475 = CARTESIAN_POINT('Ctrl Pts',(-29.9981473192967,-7.59210557221634,
15.0072731137197)) ;
#22476 = CARTESIAN_POINT('Ctrl Pts',(-29.1792583701285,-6.89610811582497,
12.86098396712)) ;
#22477 = CARTESIAN_POINT('Ctrl Pts',(-27.8122956599382,-5.73660744609276,
9.28448922209497)) ;
#22478 = CARTESIAN_POINT('Ctrl Pts',(-26.155155413787,-4.35020365083683,4.99743947373446)) ;
#22479 = CARTESIAN_POINT('Ctrl Pts',(-25.0283996405944,-3.44029824352441,
2.14308849921247)) ;
#22480 = CARTESIAN_POINT('Ctrl Pts',(-24.4500092405164,-3.00195022998226,
0.716220735767208)) ;
#22481 = CARTESIAN_POINT('Ctrl Pts',(-24.1589049321088,-2.79360243354776,
-5.70272704059072E-10)) ;
#22482 = CARTESIAN_POINT('Ctrl Pts',(-28.6654023870952,-7.59208088863895,
15.0047443273315)) ;
#22483 = CARTESIAN_POINT('Ctrl Pts',(-28.0118306429454,-6.92739322509109,
12.8579428468339)) ;
#22484 = CARTESIAN_POINT('Ctrl Pts',(-26.9205390890661,-5.81959198653294,
9.28039690179885)) ;
#22485 = CARTESIAN_POINT('Ctrl Pts',(-25.5975062439661,-4.49340440306587,
4.99035344644854)) ;
#22486 = CARTESIAN_POINT('Ctrl Pts',(-24.696887404406,-3.61843630935476,2.13290843001981)) ;
#22487 = CARTESIAN_POINT('Ctrl Pts',(-24.231863933635,-3.19121227129626,0.705454724400515)) ;
#22488 = CARTESIAN_POINT('Ctrl Pts',(-23.9940039875064,-2.98789208895153,
-0.00956374451382109)) ;
#22489 = CARTESIAN_POINT('Ctrl Pts',(-26.6659920777596,-7.59211093203314,
15.0017046656488)) ;
#22490 = CARTESIAN_POINT('Ctrl Pts',(-26.2487210328116,-6.96393546602423,
12.8542436051414)) ;
#22491 = CARTESIAN_POINT('Ctrl Pts',(-25.551936157679,-5.91719526611694,9.27528884741571)) ;
#22492 = CARTESIAN_POINT('Ctrl Pts',(-24.7073383684488,-4.66179365816894,
4.9815562676005)) ;
#22493 = CARTESIAN_POINT('Ctrl Pts',(-24.131376536521,-3.82821717034421,2.12007028295518)) ;
#22494 = CARTESIAN_POINT('Ctrl Pts',(-23.8331919862405,-3.4144691374418,0.689960097960527)) ;
#22495 = CARTESIAN_POINT('Ctrl Pts',(-23.6762514799622,-3.21253192150677,
-0.0250972881037275)) ;
#22496 = CARTESIAN_POINT('Ctrl Pts',(-23.3332927479438,-7.5921558493803,14.9995815283504)) ;
#22497 = CARTESIAN_POINT('Ctrl Pts',(-23.2961810253174,-6.98936415220679,
12.8516417322129)) ;
#22498 = CARTESIAN_POINT('Ctrl Pts',(-23.2341794813628,-5.98449411694383,
9.27170531871678)) ;
#22499 = CARTESIAN_POINT('Ctrl Pts',(-23.1590806809098,-4.7786211064264,4.975481034806)) ;
#22500 = CARTESIAN_POINT('Ctrl Pts',(-23.1077088424374,-3.97369033142903,
2.11102719571202)) ;
#22501 = CARTESIAN_POINT('Ctrl Pts',(-23.0810207228591,-3.57040548608313,
0.678584002796474)) ;
#22502 = CARTESIAN_POINT('Ctrl Pts',(-23.0663319046393,-3.36714380447418,
-0.037695190406408)) ;
#22503 = CARTESIAN_POINT('Ctrl Pts',(-20.0004784533517,-7.59212538979759,
15.0006756318296)) ;
#22504 = CARTESIAN_POINT('Ctrl Pts',(-20.3389974659838,-6.97635407369755,
12.8529859672692)) ;
#22505 = CARTESIAN_POINT('Ctrl Pts',(-20.904309853669,-5.95003859913919,9.27357788116746)) ;
#22506 = CARTESIAN_POINT('Ctrl Pts',(-21.589449075084,-4.71871053547002,4.97864159456366)) ;
#22507 = CARTESIAN_POINT('Ctrl Pts',(-22.0572141827788,-3.89911706770722,
2.11576153158121)) ;
#22508 = CARTESIAN_POINT('Ctrl Pts',(-22.2997449599209,-3.49018725280383,
0.68467274594701)) ;
#22509 = CARTESIAN_POINT('Ctrl Pts',(-22.4296586836676,-3.28819168978624,
-0.0306758267980919)) ;
#22510 = CARTESIAN_POINT('Ctrl Pts',(-17.3345976129064,-7.59208088863895,
15.0047443273315)) ;
#22511 = CARTESIAN_POINT('Ctrl Pts',(-17.9881563810077,-6.92728037248107,
12.8579470839996)) ;
#22512 = CARTESIAN_POINT('Ctrl Pts',(-19.0794572594637,-5.81968155705656,
9.28034957582959)) ;
#22513 = CARTESIAN_POINT('Ctrl Pts',(-20.4024577562282,-4.493316778673,4.99022917054663)) ;
#22514 = CARTESIAN_POINT('Ctrl Pts',(-21.3030600185225,-3.61832290138349,
2.13278098397722)) ;
#22515 = CARTESIAN_POINT('Ctrl Pts',(-21.7680877456986,-3.19093731667989,
0.705304501480531)) ;
#22516 = CARTESIAN_POINT('Ctrl Pts',(-22.0059960124938,-2.98789208895172,
-0.00956374451383244)) ;
#22517 = CARTESIAN_POINT('Ctrl Pts',(-16.0018526807048,-7.59210557221634,
15.0072731137197)) ;
#22518 = CARTESIAN_POINT('Ctrl Pts',(-16.8207416298728,-6.896108115825,12.86098396712)) ;
#22519 = CARTESIAN_POINT('Ctrl Pts',(-18.1877043400628,-5.73660744609285,
9.28448922209497)) ;
#22520 = CARTESIAN_POINT('Ctrl Pts',(-19.8448445862136,-4.350203650837,4.99743947373445)) ;
#22521 = CARTESIAN_POINT('Ctrl Pts',(-20.971600359406,-3.44029824352462,2.14308849921246)) ;
#22522 = CARTESIAN_POINT('Ctrl Pts',(-21.5499907594839,-3.00195022998247,
0.716220735767196)) ;
#22523 = CARTESIAN_POINT('Ctrl Pts',(-21.8410950678914,-2.79360243354798,
-5.70283445466835E-10)) ;
#22524 = CARTESIAN_POINT('',(-16.2137002055612,-7.58988663107372,15.)) ;
#22525 = CARTESIAN_POINT('Ctrl Pts',(-16.2137002055612,-7.58988663107372,
15.)) ;
#22526 = CARTESIAN_POINT('Ctrl Pts',(-18.478683735487,-7.59137674406499,15.)) ;
#22527 = CARTESIAN_POINT('Ctrl Pts',(-20.6776392287968,-7.59210830988921,
15.)) ;
#22528 = CARTESIAN_POINT('Ctrl Pts',(-25.2082049599243,-7.59214580234589,
15.)) ;
#22529 = CARTESIAN_POINT('Ctrl Pts',(-27.4623569795733,-7.59141553286644,
15.)) ;
#22530 = CARTESIAN_POINT('Ctrl Pts',(-29.7862997944388,-7.58988663107372,
15.)) ;
#22531 = CARTESIAN_POINT('',(-21.8072311118067,-2.82237333273713,0.089151802298673)) ;
#22532 = CARTESIAN_POINT('Ctrl Pts',(-21.8072311118067,-2.82237333273713,
0.089151802298673)) ;
#22533 = CARTESIAN_POINT('Ctrl Pts',(-21.8065429903626,-2.82295781693531,
0.0909648406217181)) ;
#22534 = CARTESIAN_POINT('Ctrl Pts',(-21.8058548888846,-2.82354227570887,
0.0927779127895756)) ;
#22535 = CARTESIAN_POINT('Ctrl Pts',(-21.8051668182352,-2.82412669991061,
0.0945909897307087)) ;
#22536 = CARTESIAN_POINT('Ctrl Pts',(-21.3321463194345,-3.22589449435074,
1.34100741448435)) ;
#22537 = CARTESIAN_POINT('Ctrl Pts',(-20.9412685773966,-3.55537108960553,
2.39676636675827)) ;
#22538 = CARTESIAN_POINT('Ctrl Pts',(-19.998603574444,-4.35779260496273,4.91745775519203)) ;
#22539 = CARTESIAN_POINT('Ctrl Pts',(-19.7551863923557,-4.56499578265944,
5.56835663524474)) ;
#22540 = CARTESIAN_POINT('Ctrl Pts',(-19.4750304667258,-4.80369474586863,
6.31696808781126)) ;
#22541 = CARTESIAN_POINT('Ctrl Pts',(-19.147214797811,-5.08330280289709,7.19178768834422)) ;
#22542 = CARTESIAN_POINT('Ctrl Pts',(-19.0457931368179,-5.16980969155427,
7.4624448453042)) ;
#22543 = CARTESIAN_POINT('Ctrl Pts',(-18.9398048742897,-5.2602370332511,7.74519133448698)) ;
#22544 = CARTESIAN_POINT('Ctrl Pts',(-18.8343151585828,-5.35026227473964,
8.02651072809489)) ;
#22545 = CARTESIAN_POINT('Ctrl Pts',(-17.9682804998251,-6.08933886405152,
10.3360471925039)) ;
#22546 = CARTESIAN_POINT('Ctrl Pts',(-17.0532905544484,-6.87166393545832,
12.769529780144)) ;
#22547 = CARTESIAN_POINT('Ctrl Pts',(-16.2137002055612,-7.58988663107372,
15.)) ;
#22548 = CARTESIAN_POINT('',(-21.841095068034,-2.79360243342669,-4.72717753829954E-10)) ;
#22549 = CARTESIAN_POINT('Ctrl Pts',(-21.84109506789,-2.79360243354897,-5.66911864674502E-10)) ;
#22550 = CARTESIAN_POINT('Ctrl Pts',(-21.8304825380899,-2.8026212118579,0.0279159123264755)) ;
#22551 = CARTESIAN_POINT('Ctrl Pts',(-21.8198816239617,-2.81162928529328,
0.0558291551528413)) ;
#22552 = CARTESIAN_POINT('Ctrl Pts',(-21.8093004558439,-2.8206195620731,0.0837151694762296)) ;
#22553 = CARTESIAN_POINT('Ctrl Pts',(-21.8086125788215,-2.82120401595886,
0.0855280268363439)) ;
#22554 = CARTESIAN_POINT('Ctrl Pts',(-21.8079247354895,-2.82178843693437,
0.0873409002953505)) ;
#22555 = CARTESIAN_POINT('Ctrl Pts',(-21.8072369214027,-2.82237282873864,
0.0891538007783507)) ;
#22556 = CARTESIAN_POINT('Ctrl Pts',(-24.1589049323255,-2.79360243373209,
-2.99383723405346E-18)) ;
#22557 = CARTESIAN_POINT('Ctrl Pts',(-24.041059962996,-2.93783796856924,-2.86693616357875E-18)) ;
#22558 = CARTESIAN_POINT('Ctrl Pts',(-23.8975075094909,-3.05863551376881,
-1.87079518543243E-12)) ;
#22559 = CARTESIAN_POINT('Ctrl Pts',(-23.5658814904478,-3.24512334221452,
-1.87079518543243E-12)) ;
#22560 = CARTESIAN_POINT('Ctrl Pts',(-23.3797263777628,-3.30630896980136,
-6.13256942631573E-14)) ;
#22561 = CARTESIAN_POINT('Ctrl Pts',(-22.9929117798555,-3.35479334786308,
-6.13261965942139E-14)) ;
#22562 = CARTESIAN_POINT('Ctrl Pts',(-22.7955456606775,-3.34100668814767,
-1.18465996779747E-16)) ;
#22563 = CARTESIAN_POINT('Ctrl Pts',(-22.453795578295,-3.24835176067042,-1.17553053613156E-16)) ;
#22564 = CARTESIAN_POINT('Ctrl Pts',(-22.3085473875398,-3.18300649052949,
1.7646913418378E-13)) ;
#22565 = CARTESIAN_POINT('Ctrl Pts',(-22.0497655129528,-3.01274318515093,
1.76470729940071E-13)) ;
#22566 = CARTESIAN_POINT('Ctrl Pts',(-21.9368651572099,-2.91081957218221,
2.97818456042393E-17)) ;
#22567 = CARTESIAN_POINT('Ctrl Pts',(-21.8410950676745,-2.79360243373208,
2.97352861784956E-17)) ;
#22568 = CARTESIAN_POINT('Ctrl Pts',(-16.2120295002238,-7.79822359640593,
15.004760387006)) ;
#22569 = CARTESIAN_POINT('Ctrl Pts',(-17.2939346788131,-6.86282814397786,
12.1445710778738)) ;
#22570 = CARTESIAN_POINT('Ctrl Pts',(-18.916508261312,-5.45797832424605,7.85475085521625)) ;
#22571 = CARTESIAN_POINT('Ctrl Pts',(-20.8015458475062,-3.79067453624556,
2.85615457147683)) ;
#22572 = CARTESIAN_POINT('Ctrl Pts',(-21.5889562660143,-3.04704003130453,
0.715613732718789)) ;
#22573 = CARTESIAN_POINT('Ctrl Pts',(-21.8410950678928,-2.79360243354618,
-5.74823466603647E-10)) ;
#22574 = CARTESIAN_POINT('Ctrl Pts',(-16.2119914143525,-6.65586778828599,
15.0030622151785)) ;
#22575 = CARTESIAN_POINT('Ctrl Pts',(-17.2645413499124,-5.90571197085084,
12.1423953161895)) ;
#22576 = CARTESIAN_POINT('Ctrl Pts',(-18.8434539442202,-4.77886241298001,
7.85175076502351)) ;
#22577 = CARTESIAN_POINT('Ctrl Pts',(-20.6801468481248,-3.44148597527413,
2.8497432463707)) ;
#22578 = CARTESIAN_POINT('Ctrl Pts',(-21.4549018244985,-2.84279904912998,
0.707828841050375)) ;
#22579 = CARTESIAN_POINT('Ctrl Pts',(-21.7046665053844,-2.63588685245852,
-0.00706604194226517)) ;
#22580 = CARTESIAN_POINT('Ctrl Pts',(-16.2119015637445,-4.37088429774524,
15.0004367897856)) ;
#22581 = CARTESIAN_POINT('Ctrl Pts',(-17.2199451957636,-3.97936993493365,
12.1389905639006)) ;
#22582 = CARTESIAN_POINT('Ctrl Pts',(-18.7323433798125,-3.39144877186261,
7.8469202359414)) ;
#22583 = CARTESIAN_POINT('Ctrl Pts',(-20.4957476119421,-2.6929916740198,2.83991086222072)) ;
#22584 = CARTESIAN_POINT('Ctrl Pts',(-21.2501213955004,-2.37937043746566,
0.694489603884554)) ;
#22585 = CARTESIAN_POINT('Ctrl Pts',(-21.4999730616134,-2.2671878990079,-0.0206641948568487)) ;
#22586 = CARTESIAN_POINT('Ctrl Pts',(-16.2118565250724,-0.371717894292294,
14.9994437267388)) ;
#22587 = CARTESIAN_POINT('Ctrl Pts',(-17.2034970653009,-0.588656421028745,
12.1376935596273)) ;
#22588 = CARTESIAN_POINT('Ctrl Pts',(-18.6908746045858,-0.914396456191195,
7.84496467022684)) ;
#22589 = CARTESIAN_POINT('Ctrl Pts',(-20.4272574580087,-1.3014899842262,2.83611936781098)) ;
#22590 = CARTESIAN_POINT('Ctrl Pts',(-21.173694786691,-1.47529391663119,0.688887749999729)) ;
#22591 = CARTESIAN_POINT('Ctrl Pts',(-21.4246891608723,-1.53804477792109,
-0.0267691804533001)) ;
#22592 = CARTESIAN_POINT('Ctrl Pts',(-16.2119723714168,2.4846898842279,15.0022131292648)) ;
#22593 = CARTESIAN_POINT('Ctrl Pts',(-17.2497059688142,1.82724833732013,12.1413021811523)) ;
#22594 = CARTESIAN_POINT('Ctrl Pts',(-18.8070103620793,0.839346881044636,
7.85030531659959)) ;
#22595 = CARTESIAN_POINT('Ctrl Pts',(-20.6193140212913,-0.332972447041589,
2.84662301371282)) ;
#22596 = CARTESIAN_POINT('Ctrl Pts',(-21.3876763824965,-0.85887468237252,
0.70401123140127)) ;
#22597 = CARTESIAN_POINT('Ctrl Pts',(-21.6364522241304,-1.04297093808501,
-0.0105990626259748)) ;
#22598 = CARTESIAN_POINT('Ctrl Pts',(-16.2120295002238,4.19822359640781,15.004760387006)) ;
#22599 = CARTESIAN_POINT('Ctrl Pts',(-17.2939346788131,3.26282814397944,12.1445710778738)) ;
#22600 = CARTESIAN_POINT('Ctrl Pts',(-18.9165082613121,1.85797832424717,7.85475085521625)) ;
#22601 = CARTESIAN_POINT('Ctrl Pts',(-20.8015458475064,0.190674536246134,
2.85615457147684)) ;
#22602 = CARTESIAN_POINT('Ctrl Pts',(-21.5889562660145,-0.552959968695133,
0.715613732718802)) ;
#22603 = CARTESIAN_POINT('Ctrl Pts',(-21.8410950678931,-0.806397566453563,
-5.74811837017464E-10)) ;
#22604 = CARTESIAN_POINT('',(-16.2137002055612,3.98988663107372,15.)) ;
#22605 = CARTESIAN_POINT('Ctrl Pts',(-16.2137002055612,3.98988663107372,15.)) ;
#22606 = CARTESIAN_POINT('Ctrl Pts',(-16.2125145547255,2.07140621568792,15.)) ;
#22607 = CARTESIAN_POINT('Ctrl Pts',(-16.2119115973002,0.183463303037694,
15.)) ;
#22608 = CARTESIAN_POINT('Ctrl Pts',(-16.2118809961308,-3.68622209538906,
15.)) ;
#22609 = CARTESIAN_POINT('Ctrl Pts',(-16.2124839012804,-5.62180642421694,
15.)) ;
#22610 = CARTESIAN_POINT('Ctrl Pts',(-16.2137002055612,-7.58988663107371,
15.)) ;
#22611 = CARTESIAN_POINT('',(-21.8072311118067,-0.77762666726287,0.089151802298673)) ;
#22612 = CARTESIAN_POINT('Ctrl Pts',(-21.8072311118067,-0.77762666726287,
0.089151802298673)) ;
#22613 = CARTESIAN_POINT('Ctrl Pts',(-21.8065429885505,-0.777042181525532,
0.0909648453961011)) ;
#22614 = CARTESIAN_POINT('Ctrl Pts',(-21.805854890698,-0.776457725828476,
0.0927779080151138)) ;
#22615 = CARTESIAN_POINT('Ctrl Pts',(-21.8051668182363,-0.775873300088152,
0.0945909897307308)) ;
#22616 = CARTESIAN_POINT('Ctrl Pts',(-21.3321456286191,-0.374104918924787,
1.34100923475312)) ;
#22617 = CARTESIAN_POINT('Ctrl Pts',(-20.9412686792828,-0.0446289960646136,
2.3967660917748)) ;
#22618 = CARTESIAN_POINT('Ctrl Pts',(-19.9986040235856,0.757792222641507,
4.91745655418507)) ;
#22619 = CARTESIAN_POINT('Ctrl Pts',(-19.7551865550768,0.964995643873722,
5.5683562007834)) ;
#22620 = CARTESIAN_POINT('Ctrl Pts',(-19.4750302004634,1.20369497249373,6.31696880020665)) ;
#22621 = CARTESIAN_POINT('Ctrl Pts',(-19.1472138763084,1.48330358888621,7.19179014749615)) ;
#22622 = CARTESIAN_POINT('Ctrl Pts',(-19.0457924000719,1.5698103201055,7.46244681083961)) ;
#22623 = CARTESIAN_POINT('Ctrl Pts',(-18.9398043540903,1.66023747714745,7.74519272193313)) ;
#22624 = CARTESIAN_POINT('Ctrl Pts',(-18.8343148546405,1.75026253412495,8.02651153864665)) ;
#22625 = CARTESIAN_POINT('Ctrl Pts',(-17.9682802857615,2.48933904709054,10.3360477618804)) ;
#22626 = CARTESIAN_POINT('Ctrl Pts',(-17.0532904562273,3.27166401948096,12.7695300410798)) ;
#22627 = CARTESIAN_POINT('Ctrl Pts',(-16.2137002055612,3.98988663107372,15.)) ;
#22628 = CARTESIAN_POINT('',(-21.841095068039,-0.806397566577556,-4.79304988060258E-10)) ;
#22629 = CARTESIAN_POINT('Ctrl Pts',(-21.841095067893,-0.806397566453594,
-5.74813162346199E-10)) ;
#22630 = CARTESIAN_POINT('Ctrl Pts',(-21.8304825311591,-0.797378782252167,
0.0279159305576807)) ;
#22631 = CARTESIAN_POINT('Ctrl Pts',(-21.8198806143693,-0.788372087620017,
0.0558294110268321)) ;
#22632 = CARTESIAN_POINT('Ctrl Pts',(-21.8092977142497,-0.779384122982931,
0.0837157785108199)) ;
#22633 = CARTESIAN_POINT('Ctrl Pts',(-21.8086097266589,-0.778799821131193,
0.0855286534849715)) ;
#22634 = CARTESIAN_POINT('Ctrl Pts',(-21.8079217617944,-0.778215549506057,
0.0873415657621646)) ;
#22635 = CARTESIAN_POINT('Ctrl Pts',(-21.8072338308928,-0.777631317536321,
0.0891544850728279)) ;
#22636 = CARTESIAN_POINT('Ctrl Pts',(-21.8410950676745,-2.79360243373211,
1.7888651467981E-16)) ;
#22637 = CARTESIAN_POINT('Ctrl Pts',(-21.716402375793,-2.6542834674913,1.78818550473223E-16)) ;
#22638 = CARTESIAN_POINT('Ctrl Pts',(-21.6191945405804,-2.49286283644828,
-1.18389961251751E-12)) ;
#22639 = CARTESIAN_POINT('Ctrl Pts',(-21.487197585082,-2.13565023378541,-1.1839008088782E-12)) ;
#22640 = CARTESIAN_POINT('Ctrl Pts',(-21.4561344460552,-1.94241064629152,
-1.40165656858926E-15)) ;
#22641 = CARTESIAN_POINT('Ctrl Pts',(-21.4688023848785,-1.57296219574121,
-1.40165656858926E-15)) ;
#22642 = CARTESIAN_POINT('Ctrl Pts',(-21.5058130688892,-1.39951177553656,
1.45716771982052E-14)) ;
#22643 = CARTESIAN_POINT('Ctrl Pts',(-21.6365692781991,-1.07876898953231,
1.45716771982052E-14)) ;
#22644 = CARTESIAN_POINT('Ctrl Pts',(-21.7274655448062,-0.933355669598461,
-1.29039860188898E-16)) ;
#22645 = CARTESIAN_POINT('Ctrl Pts',(-21.8410950676745,-0.806397566267894,
-1.29036351619964E-16)) ;
#22646 = CARTESIAN_POINT('Ctrl Pts',(-16.001852680703,3.99210557221634,15.0072731137197)) ;
#22647 = CARTESIAN_POINT('Ctrl Pts',(-16.8207416298715,3.29610811582475,12.8609839671193)) ;
#22648 = CARTESIAN_POINT('Ctrl Pts',(-18.1877024573399,2.13660628597323,9.28448888442423)) ;
#22649 = CARTESIAN_POINT('Ctrl Pts',(-19.844842964605,0.750203431437901,4.99743893001117)) ;
#22650 = CARTESIAN_POINT('Ctrl Pts',(-20.9715983994063,-0.159702216928202,
2.14308790534903)) ;
#22651 = CARTESIAN_POINT('Ctrl Pts',(-21.5499907594854,-0.598049770019083,
0.716220735762898)) ;
#22652 = CARTESIAN_POINT('Ctrl Pts',(-21.841095067893,-0.806397566453593,
-5.74812294984461E-10)) ;
#22653 = CARTESIAN_POINT('Ctrl Pts',(-16.6682251468039,3.99209323042764,15.0060087205256)) ;
#22654 = CARTESIAN_POINT('Ctrl Pts',(-17.4045039137444,3.31167027710832,12.8594663783478)) ;
#22655 = CARTESIAN_POINT('Ctrl Pts',(-18.6335549140447,2.17813825733505,9.28242868527079)) ;
#22656 = CARTESIAN_POINT('Ctrl Pts',(-20.1237719122027,0.821772347358335,
4.99388557690666)) ;
#22657 = CARTESIAN_POINT('Ctrl Pts',(-21.1374684967843,-0.0707256802637752,
2.13799104359245)) ;
#22658 = CARTESIAN_POINT('Ctrl Pts',(-21.6593105354534,-0.503423080828448,
0.710881903949976)) ;
#22659 = CARTESIAN_POINT('Ctrl Pts',(-21.9235455401941,-0.709252738751684,
-0.00478187254658313)) ;
#22660 = CARTESIAN_POINT('Ctrl Pts',(-18.6674857660828,3.99209091164725,15.0025729768987)) ;
#22661 = CARTESIAN_POINT('Ctrl Pts',(-19.1614746123909,3.35363082901585,12.855308289841)) ;
#22662 = CARTESIAN_POINT('Ctrl Pts',(-19.9863755029411,2.28972627060116,9.2767748169095)) ;
#22663 = CARTESIAN_POINT('Ctrl Pts',(-20.9863676148636,1.01425473330893,4.98409359929946)) ;
#22664 = CARTESIAN_POINT('Ctrl Pts',(-21.6680397534922,0.168983505203374,
2.12382823604792)) ;
#22665 = CARTESIAN_POINT('Ctrl Pts',(-22.0210644484083,-0.248866124683977,
0.694779644890225)) ;
#22666 = CARTESIAN_POINT('Ctrl Pts',(-22.2056967668507,-0.450222874926842,
-0.0198469372912451)) ;
#22667 = CARTESIAN_POINT('Ctrl Pts',(-22.0001427064207,3.99216271493084,14.9993531978443)) ;
#22668 = CARTESIAN_POINT('Ctrl Pts',(-22.1123412771431,3.39200499629872,12.8513619624513)) ;
#22669 = CARTESIAN_POINT('Ctrl Pts',(-22.2996679554014,2.39168358729901,9.2712991683703)) ;
#22670 = CARTESIAN_POINT('Ctrl Pts',(-22.5266934010037,1.19099399650789,4.97478325695134)) ;
#22671 = CARTESIAN_POINT('Ctrl Pts',(-22.6818522659833,0.389104720411302,
2.1100005997556)) ;
#22672 = CARTESIAN_POINT('Ctrl Pts',(-22.7622868668625,-0.013113282879768,
0.677230000874634)) ;
#22673 = CARTESIAN_POINT('Ctrl Pts',(-22.806110018343,-0.216603976952604,
-0.0391821457269935)) ;
#22674 = CARTESIAN_POINT('Ctrl Pts',(-25.9995219192719,3.99212515591032,15.0006787361289)) ;
#22675 = CARTESIAN_POINT('Ctrl Pts',(-25.6610300798093,3.37631293153872,12.85299059408)) ;
#22676 = CARTESIAN_POINT('Ctrl Pts',(-25.0957200971754,2.34995910229997,9.27358133907209)) ;
#22677 = CARTESIAN_POINT('Ctrl Pts',(-24.4106656326799,1.11857404454784,4.97865384323633)) ;
#22678 = CARTESIAN_POINT('Ctrl Pts',(-23.9429141916785,0.298927109368283,
2.11577890293457)) ;
#22679 = CARTESIAN_POINT('Ctrl Pts',(-23.7004725142412,-0.109962398029831,
0.684723933467854)) ;
#22680 = CARTESIAN_POINT('Ctrl Pts',(-23.5704121779659,-0.311946932728745,
-0.030647716704717)) ;
#22681 = CARTESIAN_POINT('Ctrl Pts',(-28.6654023870944,3.99208088863895,15.0047443273315)) ;
#22682 = CARTESIAN_POINT('Ctrl Pts',(-28.0118267664842,3.32730856489621,12.8579460343649)) ;
#22683 = CARTESIAN_POINT('Ctrl Pts',(-26.9205516217294,2.21967036822145,9.28035754568041)) ;
#22684 = CARTESIAN_POINT('Ctrl Pts',(-25.5975051802046,0.893334293744912,
4.99023689930695)) ;
#22685 = CARTESIAN_POINT('Ctrl Pts',(-24.6969016254348,0.0183616639676227,
2.13278867184277)) ;
#22686 = CARTESIAN_POINT('Ctrl Pts',(-24.2318215462195,-0.409050652094805,
0.705292734981902)) ;
#22687 = CARTESIAN_POINT('Ctrl Pts',(-23.9940039875048,-0.61210791104966,
-0.00956374451836098)) ;
#22688 = CARTESIAN_POINT('Ctrl Pts',(-29.9981473192961,3.99210557221634,15.0072731137197)) ;
#22689 = CARTESIAN_POINT('Ctrl Pts',(-29.1792583701277,3.29610811582477,12.8609839671193)) ;
#22690 = CARTESIAN_POINT('Ctrl Pts',(-27.8122975426595,2.13660628597329,9.28448888442423)) ;
#22691 = CARTESIAN_POINT('Ctrl Pts',(-26.1551570353946,0.750203431438,4.99743893001117)) ;
#22692 = CARTESIAN_POINT('Ctrl Pts',(-25.0284016005935,-0.159702216928078,
2.14308790534903)) ;
#22693 = CARTESIAN_POINT('Ctrl Pts',(-24.4500092405145,-0.598049770018951,
0.71622073576289)) ;
#22694 = CARTESIAN_POINT('Ctrl Pts',(-24.1589049321068,-0.806397566453458,
-5.74818942444821E-10)) ;
#22695 = CARTESIAN_POINT('Ctrl Pts',(-29.7862997944388,3.98988663107372,15.)) ;
#22696 = CARTESIAN_POINT('Ctrl Pts',(-27.5213162645095,3.99137674406499,15.)) ;
#22697 = CARTESIAN_POINT('Ctrl Pts',(-25.3223607712015,3.99210830988921,15.)) ;
#22698 = CARTESIAN_POINT('Ctrl Pts',(-20.7917950400773,3.99214580234589,15.)) ;
#22699 = CARTESIAN_POINT('Ctrl Pts',(-18.5376430204301,3.99141553286645,15.)) ;
#22700 = CARTESIAN_POINT('Ctrl Pts',(-16.2137002055612,3.98988663107372,15.)) ;
#22701 = CARTESIAN_POINT('Ctrl Pts',(-21.8410950676745,-0.806397566267961,
2.12829438470106E-16)) ;
#22702 = CARTESIAN_POINT('Ctrl Pts',(-21.9589400370039,-0.66216203143079,
2.11480923218598E-16)) ;
#22703 = CARTESIAN_POINT('Ctrl Pts',(-22.1024924905091,-0.541364486231195,
-1.87079518543243E-12)) ;
#22704 = CARTESIAN_POINT('Ctrl Pts',(-22.4341185095522,-0.354876657785478,
-1.87079518543243E-12)) ;
#22705 = CARTESIAN_POINT('Ctrl Pts',(-22.6202736222372,-0.29369103019864,
-6.13118164753495E-14)) ;
#22706 = CARTESIAN_POINT('Ctrl Pts',(-23.0070882201445,-0.245206652136923,
-6.13123188064061E-14)) ;
#22707 = CARTESIAN_POINT('Ctrl Pts',(-23.2044543393225,-0.258993311852331,
-1.53160466299283E-16)) ;
#22708 = CARTESIAN_POINT('Ctrl Pts',(-23.546204421705,-0.35164823932958,-1.52247523132693E-16)) ;
#22709 = CARTESIAN_POINT('Ctrl Pts',(-23.6914526124602,-0.416993509470512,
1.76455256395972E-13)) ;
#22710 = CARTESIAN_POINT('Ctrl Pts',(-23.9502344870472,-0.587256814849067,
1.76456852152263E-13)) ;
#22711 = CARTESIAN_POINT('Ctrl Pts',(-24.0631348427901,-0.689180427817769,
6.92945052858629E-17)) ;
#22712 = CARTESIAN_POINT('Ctrl Pts',(-24.1589049323255,-0.806397566267902,
6.93843681060263E-17)) ;
#22713 = CARTESIAN_POINT('Origin',(-23.,-1.8,0.)) ;
#22714 = CARTESIAN_POINT('',(-24.3286990541393,-0.661115096452054,0.)) ;
#22715 = CARTESIAN_POINT('',(-24.3286990541393,-2.93888490354795,0.)) ;
#22716 = CARTESIAN_POINT('Origin',(-23.,-1.8,0.)) ;
#22717 = CARTESIAN_POINT('',(-21.6713009458607,-0.661115096452054,0.)) ;
#22718 = CARTESIAN_POINT('Origin',(-23.,-1.8,0.)) ;
#22719 = CARTESIAN_POINT('',(-21.6713009458607,-2.93888490354795,0.)) ;
#22720 = CARTESIAN_POINT('Origin',(-23.,-1.8,0.)) ;
#22721 = CARTESIAN_POINT('Origin',(-23.,-1.8,0.)) ;
#22722 = CARTESIAN_POINT('Origin',(-23.,-1.8,15.)) ;
#22723 = CARTESIAN_POINT('',(-30.,4.2,15.)) ;
#22724 = CARTESIAN_POINT('',(-30.,-7.8,15.)) ;
#22725 = CARTESIAN_POINT('',(-30.,4.2,15.)) ;
#22726 = CARTESIAN_POINT('',(-16.,-7.8,15.)) ;
#22727 = CARTESIAN_POINT('',(-30.,-7.8,15.)) ;
#22728 = CARTESIAN_POINT('',(-16.,4.2,15.)) ;
#22729 = CARTESIAN_POINT('',(-16.,-7.8,15.)) ;
#22730 = CARTESIAN_POINT('',(-16.,4.2,15.)) ;
#22731 = CARTESIAN_POINT('Ctrl Pts',(-30.,4.2,15.)) ;
#22732 = CARTESIAN_POINT('Ctrl Pts',(-28.1095663513798,2.57962830118265,10.)) ;
#22733 = CARTESIAN_POINT('Ctrl Pts',(-26.2191327027595,0.959256602365297,
5.)) ;
#22734 = CARTESIAN_POINT('Ctrl Pts',(-24.3286990541393,-0.661115096452054,
0.)) ;
#22735 = CARTESIAN_POINT('Ctrl Pts',(-30.,3.05714285714286,15.)) ;
#22736 = CARTESIAN_POINT('Ctrl Pts',(-28.1608824747724,1.75795796494175,9.99999999999999)) ;
#22737 = CARTESIAN_POINT('Ctrl Pts',(-26.3215392010018,0.458726737174903,
5.00000000000001)) ;
#22738 = CARTESIAN_POINT('Ctrl Pts',(-24.4824216757743,-0.840458155026201,
0.)) ;
#22739 = CARTESIAN_POINT('Ctrl Pts',(-30.,0.77142857142857,15.)) ;
#22740 = CARTESIAN_POINT('Ctrl Pts',(-28.2386698968374,0.0935987464520723,
10.)) ;
#22741 = CARTESIAN_POINT('Ctrl Pts',(-26.4768558425974,-0.584062875210304,
4.99999999999999)) ;
#22742 = CARTESIAN_POINT('Ctrl Pts',(-24.7155257394348,-1.2618927001868,0.)) ;
#22743 = CARTESIAN_POINT('Ctrl Pts',(-30.,-3.22857142857143,15.)) ;
#22744 = CARTESIAN_POINT('Ctrl Pts',(-28.2673008175541,-2.85300906076429,
9.99999999999999)) ;
#22745 = CARTESIAN_POINT('Ctrl Pts',(-26.5346802019186,-2.47747049404618,
5.00000000000001)) ;
#22746 = CARTESIAN_POINT('Ctrl Pts',(-24.8019810194727,-2.10190812623904,
0.)) ;
#22747 = CARTESIAN_POINT('Ctrl Pts',(-30.,-6.08571428571429,15.)) ;
#22748 = CARTESIAN_POINT('Ctrl Pts',(-28.1867947927088,-4.94728771311918,
10.)) ;
#22749 = CARTESIAN_POINT('Ctrl Pts',(-26.372488193883,-3.80829688828183,5.)) ;
#22750 = CARTESIAN_POINT('Ctrl Pts',(-24.5592829865917,-2.66987031568673,
0.)) ;
#22751 = CARTESIAN_POINT('Ctrl Pts',(-30.,-7.8,15.)) ;
#22752 = CARTESIAN_POINT('Ctrl Pts',(-28.1095663513798,-6.17962830118265,
10.)) ;
#22753 = CARTESIAN_POINT('Ctrl Pts',(-26.2191327027595,-4.5592566023653,5.)) ;
#22754 = CARTESIAN_POINT('Ctrl Pts',(-24.3286990541393,-2.93888490354795,
0.)) ;
#22755 = CARTESIAN_POINT('',(-30.,4.2,15.)) ;
#22756 = CARTESIAN_POINT('',(-30.,-7.8,15.)) ;
#22757 = CARTESIAN_POINT('Ctrl Pts',(-30.,-7.8,15.)) ;
#22758 = CARTESIAN_POINT('Ctrl Pts',(-28.1095663513798,-6.17962830118265,
10.)) ;
#22759 = CARTESIAN_POINT('Ctrl Pts',(-26.2191327027595,-4.5592566023653,5.)) ;
#22760 = CARTESIAN_POINT('Ctrl Pts',(-24.3286990541393,-2.93888490354795,
0.)) ;
#22761 = CARTESIAN_POINT('Ctrl Pts',(-28.6666666666667,-7.8,15.)) ;
#22762 = CARTESIAN_POINT('Ctrl Pts',(-27.1584336023967,-6.25242905179828,
10.)) ;
#22763 = CARTESIAN_POINT('Ctrl Pts',(-25.6499011737328,-4.70465862053891,
5.)) ;
#22764 = CARTESIAN_POINT('Ctrl Pts',(-24.1416681094628,-3.15708767233719,
0.)) ;
#22765 = CARTESIAN_POINT('Ctrl Pts',(-26.,-7.8,15.)) ;
#22766 = CARTESIAN_POINT('Ctrl Pts',(-25.2193650979419,-6.36643657871293,
10.)) ;
#22767 = CARTESIAN_POINT('Ctrl Pts',(-24.4387564842615,-4.93275627338872,
5.00000000000001)) ;
#22768 = CARTESIAN_POINT('Ctrl Pts',(-23.6581215822033,-3.49919285210164,
0.)) ;
#22769 = CARTESIAN_POINT('Ctrl Pts',(-22.,-7.8,15.)) ;
#22770 = CARTESIAN_POINT('Ctrl Pts',(-22.2587099775723,-6.40287188477929,
10.)) ;
#22771 = CARTESIAN_POINT('Ctrl Pts',(-22.5172538720266,-5.00574529287019,
4.99999999999999)) ;
#22772 = CARTESIAN_POINT('Ctrl Pts',(-22.7759638495989,-3.60861717764948,
0.)) ;
#22773 = CARTESIAN_POINT('Ctrl Pts',(-18.6666666666667,-7.8,15.)) ;
#22774 = CARTESIAN_POINT('Ctrl Pts',(-19.8062578158211,-6.31371238783143,
10.)) ;
#22775 = CARTESIAN_POINT('Ctrl Pts',(-20.9459555636257,-4.82732800860068,
5.)) ;
#22776 = CARTESIAN_POINT('Ctrl Pts',(-22.0855467127802,-3.34104039643211,
0.)) ;
#22777 = CARTESIAN_POINT('Ctrl Pts',(-16.6666666666667,-7.8,15.)) ;
#22778 = CARTESIAN_POINT('Ctrl Pts',(-18.3661025308913,-6.21593369039753,
10.)) ;
#22779 = CARTESIAN_POINT('Ctrl Pts',(-20.0653805539744,-4.63205259754504,
5.)) ;
#22780 = CARTESIAN_POINT('Ctrl Pts',(-21.764816418199,-3.04798628794257,0.)) ;
#22781 = CARTESIAN_POINT('Ctrl Pts',(-16.,-7.8,15.)) ;
#22782 = CARTESIAN_POINT('Ctrl Pts',(-17.8904336486202,-6.17962830118265,
10.)) ;
#22783 = CARTESIAN_POINT('Ctrl Pts',(-19.7808672972405,-4.5592566023653,5.)) ;
#22784 = CARTESIAN_POINT('Ctrl Pts',(-21.6713009458607,-2.93888490354795,
0.)) ;
#22785 = CARTESIAN_POINT('',(-16.,-7.8,15.)) ;
#22786 = CARTESIAN_POINT('Ctrl Pts',(-16.,-7.8,15.)) ;
#22787 = CARTESIAN_POINT('Ctrl Pts',(-17.8904336486202,-6.17962830118265,
10.)) ;
#22788 = CARTESIAN_POINT('Ctrl Pts',(-19.7808672972405,-4.5592566023653,5.)) ;
#22789 = CARTESIAN_POINT('Ctrl Pts',(-21.6713009458607,-2.93888490354795,
0.)) ;
#22790 = CARTESIAN_POINT('Ctrl Pts',(-16.,-6.65714285714286,15.)) ;
#22791 = CARTESIAN_POINT('Ctrl Pts',(-17.8391086044718,-5.35795456184796,
10.)) ;
#22792 = CARTESIAN_POINT('Ctrl Pts',(-19.678469719754,-4.0587301402687,4.99999999999999)) ;
#22793 = CARTESIAN_POINT('Ctrl Pts',(-21.5175783242257,-2.7595418449738,0.)) ;
#22794 = CARTESIAN_POINT('Ctrl Pts',(-16.,-4.37142857142857,15.)) ;
#22795 = CARTESIAN_POINT('Ctrl Pts',(-17.7613419010902,-3.69360594086809,
9.99999999999998)) ;
#22796 = CARTESIAN_POINT('Ctrl Pts',(-19.5231801272942,-3.01597519408864,
5.00000000000002)) ;
#22797 = CARTESIAN_POINT('Ctrl Pts',(-21.2845220283845,-2.33815256352815,
0.)) ;
#22798 = CARTESIAN_POINT('Ctrl Pts',(-16.,-0.371428571428572,15.)) ;
#22799 = CARTESIAN_POINT('Ctrl Pts',(-17.732695160094,-0.746986389367562,
10.)) ;
#22800 = CARTESIAN_POINT('Ctrl Pts',(-19.4652823817506,-1.12245808880451,
4.99999999999999)) ;
#22801 = CARTESIAN_POINT('Ctrl Pts',(-21.1979775418446,-1.4980159067435,0.)) ;
#22802 = CARTESIAN_POINT('Ctrl Pts',(-16.,2.48571428571428,15.)) ;
#22803 = CARTESIAN_POINT('Ctrl Pts',(-17.8132062724847,1.34728533115534,9.99999999999999)) ;
#22804 = CARTESIAN_POINT('Ctrl Pts',(-19.6275107409235,0.208299270245674,
5.00000000000001)) ;
#22805 = CARTESIAN_POINT('Ctrl Pts',(-21.4407170134083,-0.930129684313275,
0.)) ;
#22806 = CARTESIAN_POINT('Ctrl Pts',(-16.,4.2,15.)) ;
#22807 = CARTESIAN_POINT('Ctrl Pts',(-17.8904336486202,2.57962830118265,10.)) ;
#22808 = CARTESIAN_POINT('Ctrl Pts',(-19.7808672972405,0.959256602365297,
5.)) ;
#22809 = CARTESIAN_POINT('Ctrl Pts',(-21.6713009458607,-0.661115096452054,
0.)) ;
#22810 = CARTESIAN_POINT('',(-16.,4.2,15.)) ;
#22811 = CARTESIAN_POINT('Ctrl Pts',(-16.,4.2,15.)) ;
#22812 = CARTESIAN_POINT('Ctrl Pts',(-17.8904336486202,2.57962830118265,10.)) ;
#22813 = CARTESIAN_POINT('Ctrl Pts',(-19.7808672972405,0.959256602365298,
5.)) ;
#22814 = CARTESIAN_POINT('Ctrl Pts',(-21.6713009458607,-0.661115096452054,
0.)) ;
#22815 = CARTESIAN_POINT('Ctrl Pts',(-17.3333333333333,4.2,15.)) ;
#22816 = CARTESIAN_POINT('Ctrl Pts',(-18.8415663976033,2.65242905179828,10.)) ;
#22817 = CARTESIAN_POINT('Ctrl Pts',(-20.3500988262672,1.10465862053891,5.)) ;
#22818 = CARTESIAN_POINT('Ctrl Pts',(-21.8583318905372,-0.442912327662807,
0.)) ;
#22819 = CARTESIAN_POINT('Ctrl Pts',(-20.,4.2,15.)) ;
#22820 = CARTESIAN_POINT('Ctrl Pts',(-20.7806349020582,2.76643657871293,9.99999999999999)) ;
#22821 = CARTESIAN_POINT('Ctrl Pts',(-21.5612412315327,1.33275849418373,5.00000000000001)) ;
#22822 = CARTESIAN_POINT('Ctrl Pts',(-22.3418761335909,-0.100804927103342,
0.)) ;
#22823 = CARTESIAN_POINT('Ctrl Pts',(-24.,4.2,15.)) ;
#22824 = CARTESIAN_POINT('Ctrl Pts',(-23.7412900224277,2.80287188477929,10.)) ;
#22825 = CARTESIAN_POINT('Ctrl Pts',(-23.4827448088328,1.40574635303797,4.99999999999999)) ;
#22826 = CARTESIAN_POINT('Ctrl Pts',(-23.2240348312605,0.00861823781726209,
0.)) ;
#22827 = CARTESIAN_POINT('Ctrl Pts',(-27.3333333333333,4.2,15.)) ;
#22828 = CARTESIAN_POINT('Ctrl Pts',(-26.1937421841789,2.71371238783143,10.)) ;
#22829 = CARTESIAN_POINT('Ctrl Pts',(-25.054043528944,1.22732858634997,5.)) ;
#22830 = CARTESIAN_POINT('Ctrl Pts',(-23.9144523797896,-0.258959025818595,
0.)) ;
#22831 = CARTESIAN_POINT('Ctrl Pts',(-29.3333333333333,4.2,15.)) ;
#22832 = CARTESIAN_POINT('Ctrl Pts',(-27.6338974691087,2.61593369039753,10.)) ;
#22833 = CARTESIAN_POINT('Ctrl Pts',(-25.9346194460256,1.03205259754504,5.)) ;
#22834 = CARTESIAN_POINT('Ctrl Pts',(-24.235183581801,-0.55201371205743,0.)) ;
#22835 = CARTESIAN_POINT('Ctrl Pts',(-30.,4.2,15.)) ;
#22836 = CARTESIAN_POINT('Ctrl Pts',(-28.1095663513798,2.57962830118265,10.)) ;
#22837 = CARTESIAN_POINT('Ctrl Pts',(-26.2191327027595,0.959256602365298,
5.)) ;
#22838 = CARTESIAN_POINT('Ctrl Pts',(-24.3286990541393,-0.661115096452054,
0.)) ;
#22839 = CARTESIAN_POINT('',(0.,0.,0.)) ;
#22840 = CARTESIAN_POINT('Origin',(-23.,-1.8,15.9)) ;
#22841 = CARTESIAN_POINT('',(-23.7,-1.8,16.5)) ;
#22842 = CARTESIAN_POINT('Origin',(-23.,-1.8,16.5)) ;
#22843 = CARTESIAN_POINT('',(-23.7,-1.8,15.3)) ;
#22844 = CARTESIAN_POINT('',(-23.7,-1.8,15.9)) ;
#22845 = CARTESIAN_POINT('Origin',(-23.,-1.8,15.3)) ;
#22846 = CARTESIAN_POINT('Origin',(-23.,-1.8,16.5)) ;
#22847 = CARTESIAN_POINT('Origin',(-23.,3.4,14.75)) ;
#22848 = CARTESIAN_POINT('',(-16.8,3.4,14.6)) ;
#22849 = CARTESIAN_POINT('',(-29.2,3.4,14.6)) ;
#22850 = CARTESIAN_POINT('',(-23.,3.4,14.6)) ;
#22851 = CARTESIAN_POINT('',(-16.8,3.4,15.)) ;
#22852 = CARTESIAN_POINT('',(-16.8,3.4,14.75)) ;
#22853 = CARTESIAN_POINT('',(-29.2,3.4,15.)) ;
#22854 = CARTESIAN_POINT('',(-23.,3.4,15.)) ;
#22855 = CARTESIAN_POINT('',(-29.2,3.4,14.75)) ;
#22856 = CARTESIAN_POINT('Origin',(-29.2,-1.8,14.75)) ;
#22857 = CARTESIAN_POINT('',(-29.2,-7.,14.6)) ;
#22858 = CARTESIAN_POINT('',(-29.2,-1.8,14.6)) ;
#22859 = CARTESIAN_POINT('',(-29.2,-7.,15.)) ;
#22860 = CARTESIAN_POINT('',(-29.2,-1.8,15.)) ;
#22861 = CARTESIAN_POINT('',(-29.2,-7.,14.75)) ;
#22862 = CARTESIAN_POINT('Origin',(-23.,-1.8,15.)) ;
#22863 = CARTESIAN_POINT('',(-16.8,-7.,15.)) ;
#22864 = CARTESIAN_POINT('',(-16.8,-1.8,15.)) ;
#22865 = CARTESIAN_POINT('',(-23.,-7.,15.)) ;
#22866 = CARTESIAN_POINT('Origin',(-23.,-7.,14.75)) ;
#22867 = CARTESIAN_POINT('',(-16.8,-7.,14.6)) ;
#22868 = CARTESIAN_POINT('',(-23.,-7.,14.6)) ;
#22869 = CARTESIAN_POINT('',(-16.8,-7.,14.75)) ;
#22870 = CARTESIAN_POINT('Origin',(-16.8,-1.8,14.75)) ;
#22871 = CARTESIAN_POINT('',(-16.8,-1.8,14.6)) ;
#22872 = CARTESIAN_POINT('Origin',(-23.,-1.8,14.6)) ;
#22873 = CARTESIAN_POINT('',(-16.6,3.6,14.6)) ;
#22874 = CARTESIAN_POINT('',(-16.6,-7.2,14.6)) ;
#22875 = CARTESIAN_POINT('',(-16.6,-1.8,14.6)) ;
#22876 = CARTESIAN_POINT('',(-29.4,-7.2,14.6)) ;
#22877 = CARTESIAN_POINT('',(-23.,-7.2,14.6)) ;
#22878 = CARTESIAN_POINT('',(-29.4,3.6,14.6)) ;
#22879 = CARTESIAN_POINT('',(-29.4,-1.8,14.6)) ;
#22880 = CARTESIAN_POINT('',(-23.,3.6,14.6)) ;
#22881 = CARTESIAN_POINT('Origin',(-23.,-7.2,14.8)) ;
#22882 = CARTESIAN_POINT('',(-29.4,-7.2,15.)) ;
#22883 = CARTESIAN_POINT('',(-29.4,-7.2,14.8)) ;
#22884 = CARTESIAN_POINT('',(-16.6,-7.2,15.)) ;
#22885 = CARTESIAN_POINT('',(-16.6,-7.2,14.8)) ;
#22886 = CARTESIAN_POINT('',(-23.,-7.2,15.)) ;
#22887 = CARTESIAN_POINT('Origin',(-29.4,-1.8,14.8)) ;
#22888 = CARTESIAN_POINT('',(-29.4,3.6,15.)) ;
#22889 = CARTESIAN_POINT('',(-29.4,3.6,14.8)) ;
#22890 = CARTESIAN_POINT('',(-29.4,-1.8,15.)) ;
#22891 = CARTESIAN_POINT('Origin',(-23.,3.6,14.8)) ;
#22892 = CARTESIAN_POINT('',(-16.6,3.6,15.)) ;
#22893 = CARTESIAN_POINT('',(-16.6,3.6,14.8)) ;
#22894 = CARTESIAN_POINT('',(-23.,3.6,15.)) ;
#22895 = CARTESIAN_POINT('Origin',(-16.6,-1.8,14.8)) ;
#22896 = CARTESIAN_POINT('',(-16.6,-1.8,15.)) ;
#22897 = CARTESIAN_POINT('Origin',(-23.,-1.8,15.3)) ;
#22898 = CARTESIAN_POINT('',(-15.7,-8.1,15.3)) ;
#22899 = CARTESIAN_POINT('',(-15.7,4.5,15.3)) ;
#22900 = CARTESIAN_POINT('',(-15.7,-1.8,15.3)) ;
#22901 = CARTESIAN_POINT('',(-30.3,4.5,15.3)) ;
#22902 = CARTESIAN_POINT('',(-23.,4.5,15.3)) ;
#22903 = CARTESIAN_POINT('',(-30.3,-8.1,15.3)) ;
#22904 = CARTESIAN_POINT('',(-30.3,-1.8,15.3)) ;
#22905 = CARTESIAN_POINT('',(-23.,-8.1,15.3)) ;
#22906 = CARTESIAN_POINT('Origin',(-23.,-1.8,15.)) ;
#22907 = CARTESIAN_POINT('',(-15.7,4.5,15.)) ;
#22908 = CARTESIAN_POINT('',(-15.7,-8.1,15.)) ;
#22909 = CARTESIAN_POINT('',(-15.7,-1.8,15.)) ;
#22910 = CARTESIAN_POINT('',(-30.3,-8.1,15.)) ;
#22911 = CARTESIAN_POINT('',(-23.,-8.1,15.)) ;
#22912 = CARTESIAN_POINT('',(-30.3,4.5,15.)) ;
#22913 = CARTESIAN_POINT('',(-30.3,-1.8,15.)) ;
#22914 = CARTESIAN_POINT('',(-23.,4.5,15.)) ;
#22915 = CARTESIAN_POINT('Origin',(-23.,-8.1,15.15)) ;
#22916 = CARTESIAN_POINT('',(-30.3,-8.1,15.15)) ;
#22917 = CARTESIAN_POINT('',(-15.7,-8.1,15.15)) ;
#22918 = CARTESIAN_POINT('Origin',(-30.3,-1.8,15.15)) ;
#22919 = CARTESIAN_POINT('',(-30.3,4.5,15.15)) ;
#22920 = CARTESIAN_POINT('Origin',(-23.,4.5,15.15)) ;
#22921 = CARTESIAN_POINT('',(-15.7,4.5,15.15)) ;
#22922 = CARTESIAN_POINT('Origin',(-15.7,-1.8,15.15)) ;
#22923 = CARTESIAN_POINT('',(0.,0.,0.)) ;
#22924 = CARTESIAN_POINT('Origin',(-24.4,-1.8,-0.85)) ;
#22925 = CARTESIAN_POINT('',(-24.4,-2.93137084989848,-0.6)) ;
#22926 = CARTESIAN_POINT('',(-24.4,-2.93137084989848,-1.)) ;
#22927 = CARTESIAN_POINT('',(-24.4,-2.93137084989848,-0.45)) ;
#22928 = CARTESIAN_POINT('',(-24.4,-3.2,-0.6)) ;
#22929 = CARTESIAN_POINT('',(-24.4,-1.8,-0.6)) ;
#22930 = CARTESIAN_POINT('',(-24.4,-3.2,-1.1)) ;
#22931 = CARTESIAN_POINT('',(-24.4,-3.2,-0.85)) ;
#22932 = CARTESIAN_POINT('',(-24.4,-0.4,-1.1)) ;
#22933 = CARTESIAN_POINT('',(-24.4,-1.8,-1.1)) ;
#22934 = CARTESIAN_POINT('',(-24.4,-0.4,-0.6)) ;
#22935 = CARTESIAN_POINT('',(-24.4,-0.4,-0.85)) ;
#22936 = CARTESIAN_POINT('',(-24.4,-0.668629150101522,-0.6)) ;
#22937 = CARTESIAN_POINT('',(-24.4,-1.8,-0.6)) ;
#22938 = CARTESIAN_POINT('',(-24.4,-0.668629150101522,-1.)) ;
#22939 = CARTESIAN_POINT('',(-24.4,-0.668629150101522,-0.45)) ;
#22940 = CARTESIAN_POINT('',(-24.4,-1.8,-1.)) ;
#22941 = CARTESIAN_POINT('Origin',(-23.,-1.8,-1.1)) ;
#22942 = CARTESIAN_POINT('',(-21.8381049961378,-3.2,-1.1)) ;
#22943 = CARTESIAN_POINT('',(-21.8381049961378,-0.4,-1.1)) ;
#22944 = CARTESIAN_POINT('',(-21.8381049961378,-1.8,-1.1)) ;
#22945 = CARTESIAN_POINT('',(-21.6,-3.2,-1.1)) ;
#22946 = CARTESIAN_POINT('',(-23.,-3.2,-1.1)) ;
#22947 = CARTESIAN_POINT('',(-21.6,-0.4,-1.1)) ;
#22948 = CARTESIAN_POINT('',(-21.6,-1.8,-1.1)) ;
#22949 = CARTESIAN_POINT('',(-23.,-0.4,-1.1)) ;
#22950 = CARTESIAN_POINT('Origin',(-23.,-3.2,-0.85)) ;
#22951 = CARTESIAN_POINT('',(-21.9416994755742,-3.2,-1.)) ;
#22952 = CARTESIAN_POINT('Origin',(-23.,-3.2,-2.2)) ;
#22953 = CARTESIAN_POINT('',(-21.8686291501015,-3.2,-1.)) ;
#22954 = CARTESIAN_POINT('',(-23.,-3.2,-1.)) ;
#22955 = CARTESIAN_POINT('',(-21.8686291501015,-3.2,-0.6)) ;
#22956 = CARTESIAN_POINT('',(-21.8686291501015,-3.2,-0.45)) ;
#22957 = CARTESIAN_POINT('',(-21.6,-3.2,-0.6)) ;
#22958 = CARTESIAN_POINT('',(-23.,-3.2,-0.6)) ;
#22959 = CARTESIAN_POINT('',(-21.6,-3.2,-0.85)) ;
#22960 = CARTESIAN_POINT('Origin',(-23.,-0.4,-0.85)) ;
#22961 = CARTESIAN_POINT('',(-21.9416994755742,-0.4,-1.)) ;
#22962 = CARTESIAN_POINT('Origin',(-23.,-0.4,-2.2)) ;
#22963 = CARTESIAN_POINT('',(-21.6,-0.4,-0.6)) ;
#22964 = CARTESIAN_POINT('',(-21.6,-0.4,-0.85)) ;
#22965 = CARTESIAN_POINT('',(-21.8686291501015,-0.4,-0.6)) ;
#22966 = CARTESIAN_POINT('',(-23.,-0.4,-0.6)) ;
#22967 = CARTESIAN_POINT('',(-21.8686291501015,-0.4,-1.)) ;
#22968 = CARTESIAN_POINT('',(-21.8686291501015,-0.4,-0.45)) ;
#22969 = CARTESIAN_POINT('',(-23.,-0.4,-1.)) ;
#22970 = CARTESIAN_POINT('Origin',(-23.,-0.4,-0.85)) ;
#22971 = CARTESIAN_POINT('',(-24.1313708498985,-0.4,-0.6)) ;
#22972 = CARTESIAN_POINT('',(-24.1313708498985,-0.4,-1.)) ;
#22973 = CARTESIAN_POINT('',(-24.1313708498985,-0.4,-0.45)) ;
#22974 = CARTESIAN_POINT('',(-23.,-0.4,-0.6)) ;
#22975 = CARTESIAN_POINT('',(-24.1618950038622,-0.4,-1.1)) ;
#22976 = CARTESIAN_POINT('',(-23.,-0.4,-1.1)) ;
#22977 = CARTESIAN_POINT('',(-24.0583005244258,-0.4,-1.)) ;
#22978 = CARTESIAN_POINT('Origin',(-23.,-0.4,-2.2)) ;
#22979 = CARTESIAN_POINT('',(-23.,-0.4,-1.)) ;
#22980 = CARTESIAN_POINT('Origin',(-23.,-1.8,-0.6)) ;
#22981 = CARTESIAN_POINT('',(-21.6,-0.668629150101522,-0.6)) ;
#22982 = CARTESIAN_POINT('Origin',(-23.,-1.8,-0.6)) ;
#22983 = CARTESIAN_POINT('',(-21.6,-1.8,-0.6)) ;
#22984 = CARTESIAN_POINT('Origin',(-23.,-1.8,-0.6)) ;
#22985 = CARTESIAN_POINT('Origin',(-23.,-1.8,-0.6)) ;
#22986 = CARTESIAN_POINT('Origin',(-23.,-1.8,-0.6)) ;
#22987 = CARTESIAN_POINT('',(-21.6,-2.93137084989848,-0.6)) ;
#22988 = CARTESIAN_POINT('Origin',(-23.,-1.8,-0.6)) ;
#22989 = CARTESIAN_POINT('',(-21.6,-1.8,-0.6)) ;
#22990 = CARTESIAN_POINT('Origin',(-23.,-1.8,-0.6)) ;
#22991 = CARTESIAN_POINT('',(-24.1313708498985,-3.2,-0.6)) ;
#22992 = CARTESIAN_POINT('Origin',(-23.,-1.8,-0.6)) ;
#22993 = CARTESIAN_POINT('',(-23.,-3.2,-0.6)) ;
#22994 = CARTESIAN_POINT('Origin',(-23.,-1.8,-1.1)) ;
#22995 = CARTESIAN_POINT('',(-24.1618950038622,-3.2,-1.1)) ;
#22996 = CARTESIAN_POINT('',(-24.1618950038622,-1.8,-1.1)) ;
#22997 = CARTESIAN_POINT('',(-23.,-3.2,-1.1)) ;
#22998 = CARTESIAN_POINT('Origin',(-23.,-3.2,-0.85)) ;
#22999 = CARTESIAN_POINT('',(-24.1313708498985,-3.2,-1.)) ;
#23000 = CARTESIAN_POINT('',(-24.1313708498985,-3.2,-0.45)) ;
#23001 = CARTESIAN_POINT('',(-24.0583005244258,-3.2,-1.)) ;
#23002 = CARTESIAN_POINT('',(-23.,-3.2,-1.)) ;
#23003 = CARTESIAN_POINT('Origin',(-23.,-3.2,-2.2)) ;
#23004 = CARTESIAN_POINT('Origin',(-21.6,-1.8,-0.85)) ;
#23005 = CARTESIAN_POINT('',(-21.6,-2.93137084989848,-1.)) ;
#23006 = CARTESIAN_POINT('',(-21.6,-2.93137084989848,-0.45)) ;
#23007 = CARTESIAN_POINT('',(-21.6,-0.668629150101522,-1.)) ;
#23008 = CARTESIAN_POINT('',(-21.6,-1.8,-1.)) ;
#23009 = CARTESIAN_POINT('',(-21.6,-0.668629150101522,-0.45)) ;
#23010 = CARTESIAN_POINT('Origin',(-23.,-1.8,-1.)) ;
#23011 = CARTESIAN_POINT('',(-24.0583005244258,-0.343978022143896,-1.)) ;
#23012 = CARTESIAN_POINT('',(-24.0583005244258,-1.8,-1.)) ;
#23013 = CARTESIAN_POINT('Origin',(-23.,-1.8,-1.)) ;
#23014 = CARTESIAN_POINT('Origin',(-23.,-1.8,-1.)) ;
#23015 = CARTESIAN_POINT('',(-24.0583005244258,-3.2560219778561,-1.)) ;
#23016 = CARTESIAN_POINT('Origin',(-23.,-1.8,-1.)) ;
#23017 = CARTESIAN_POINT('',(-24.0583005244258,-1.8,-1.)) ;
#23018 = CARTESIAN_POINT('Origin',(-23.,-1.8,-1.)) ;
#23019 = CARTESIAN_POINT('',(-24.8,-1.8,-1.)) ;
#23020 = CARTESIAN_POINT('Origin',(-23.,-1.8,-1.)) ;
#23021 = CARTESIAN_POINT('Origin',(-23.,-1.8,-1.)) ;
#23022 = CARTESIAN_POINT('Origin',(-23.,-1.8,-1.)) ;
#23023 = CARTESIAN_POINT('',(-21.9416994755742,-0.343978022143896,-1.)) ;
#23024 = CARTESIAN_POINT('Origin',(-23.,-1.8,-1.)) ;
#23025 = CARTESIAN_POINT('',(-21.9416994755742,-1.8,-1.)) ;
#23026 = CARTESIAN_POINT('Origin',(-23.,-1.8,-1.)) ;
#23027 = CARTESIAN_POINT('Origin',(-23.,-1.8,-1.)) ;
#23028 = CARTESIAN_POINT('Origin',(-23.,-1.8,-3.4)) ;
#23029 = CARTESIAN_POINT('',(-24.3,-1.8,-4.5)) ;
#23030 = CARTESIAN_POINT('Origin',(-23.,-1.8,-4.5)) ;
#23031 = CARTESIAN_POINT('',(-24.3,-1.8,-3.13273790530888)) ;
#23032 = CARTESIAN_POINT('',(-24.3,-1.8,-3.4)) ;
#23033 = CARTESIAN_POINT('',(-21.7,-1.8,-3.13273790530888)) ;
#23034 = CARTESIAN_POINT('Ctrl Pts',(-21.7,-1.8,-3.13273790530888)) ;
#23035 = CARTESIAN_POINT('Ctrl Pts',(-21.7,-1.88934386696009,-3.13273790530888)) ;
#23036 = CARTESIAN_POINT('Ctrl Pts',(-21.7092429454133,-1.97758308210185,
-3.14593464346712)) ;
#23037 = CARTESIAN_POINT('Ctrl Pts',(-21.7444789059789,-2.14821877213838,
-3.19222623476834)) ;
#23038 = CARTESIAN_POINT('Ctrl Pts',(-21.7704660290006,-2.23068508647083,
-3.22506776421433)) ;
#23039 = CARTESIAN_POINT('Ctrl Pts',(-21.8704353089628,-2.46562551307362,
-3.33760910141692)) ;
#23040 = CARTESIAN_POINT('Ctrl Pts',(-21.9675840369442,-2.60606166802919,
-3.43013719509726)) ;
#23041 = CARTESIAN_POINT('Ctrl Pts',(-22.1900504239759,-2.82852805506094,
-3.58629392075118)) ;
#23042 = CARTESIAN_POINT('Ctrl Pts',(-22.3305352921443,-2.92774057937871,
-3.66289157340511)) ;
#23043 = CARTESIAN_POINT('Ctrl Pts',(-22.5694255964999,-3.02967523999069,
-3.74326420954647)) ;
#23044 = CARTESIAN_POINT('Ctrl Pts',(-22.6537071359882,-3.05610474843748,
-3.76450988863227)) ;
#23045 = CARTESIAN_POINT('Ctrl Pts',(-22.8258541681822,-3.09127499629695,
-3.79288517120475)) ;
#23046 = CARTESIAN_POINT('Ctrl Pts',(-22.9137253103631,-3.1,-3.8)) ;
#23047 = CARTESIAN_POINT('Ctrl Pts',(-23.0862746896369,-3.1,-3.8)) ;
#23048 = CARTESIAN_POINT('Ctrl Pts',(-23.1741458318178,-3.09127499629695,
-3.79288517120475)) ;
#23049 = CARTESIAN_POINT('Ctrl Pts',(-23.3462928640118,-3.05610474843748,
-3.76450988863227)) ;
#23050 = CARTESIAN_POINT('Ctrl Pts',(-23.4305744035001,-3.02967523999069,
-3.74326420954647)) ;
#23051 = CARTESIAN_POINT('Ctrl Pts',(-23.6694647078557,-2.92774057937871,
-3.66289157340511)) ;
#23052 = CARTESIAN_POINT('Ctrl Pts',(-23.8099495760241,-2.82852805506094,
-3.58629392075118)) ;
#23053 = CARTESIAN_POINT('Ctrl Pts',(-24.0324159630558,-2.60606166802919,
-3.43013719509726)) ;
#23054 = CARTESIAN_POINT('Ctrl Pts',(-24.1295646910372,-2.46562551307362,
-3.33760910141692)) ;
#23055 = CARTESIAN_POINT('Ctrl Pts',(-24.2295339709994,-2.23068508647083,
-3.22506776421433)) ;
#23056 = CARTESIAN_POINT('Ctrl Pts',(-24.2555210940211,-2.14821877213838,
-3.19222623476834)) ;
#23057 = CARTESIAN_POINT('Ctrl Pts',(-24.2907570545867,-1.97758308210185,
-3.14593464346712)) ;
#23058 = CARTESIAN_POINT('Ctrl Pts',(-24.3,-1.88934386696009,-3.13273790530888)) ;
#23059 = CARTESIAN_POINT('Ctrl Pts',(-24.3,-1.8,-3.13273790530888)) ;
#23060 = CARTESIAN_POINT('Ctrl Pts',(-24.3,-1.8,-3.13273790530888)) ;
#23061 = CARTESIAN_POINT('Ctrl Pts',(-24.3,-1.71065613303991,-3.13273790530888)) ;
#23062 = CARTESIAN_POINT('Ctrl Pts',(-24.2907570545867,-1.62241691789815,
-3.14593464346712)) ;
#23063 = CARTESIAN_POINT('Ctrl Pts',(-24.2555210940211,-1.45178122786162,
-3.19222623476834)) ;
#23064 = CARTESIAN_POINT('Ctrl Pts',(-24.2295339709994,-1.36931491352917,
-3.22506776421433)) ;
#23065 = CARTESIAN_POINT('Ctrl Pts',(-24.1295646910372,-1.13437448692638,
-3.33760910141692)) ;
#23066 = CARTESIAN_POINT('Ctrl Pts',(-24.0324159630558,-0.993938331970815,
-3.43013719509726)) ;
#23067 = CARTESIAN_POINT('Ctrl Pts',(-23.8099495760241,-0.771471944939062,
-3.58629392075118)) ;
#23068 = CARTESIAN_POINT('Ctrl Pts',(-23.6694647078557,-0.672259420621293,
-3.66289157340511)) ;
#23069 = CARTESIAN_POINT('Ctrl Pts',(-23.4305744035001,-0.57032476000931,
-3.74326420954647)) ;
#23070 = CARTESIAN_POINT('Ctrl Pts',(-23.3462928640118,-0.543895251562523,
-3.76450988863227)) ;
#23071 = CARTESIAN_POINT('Ctrl Pts',(-23.1741458318178,-0.508725003703049,
-3.79288517120475)) ;
#23072 = CARTESIAN_POINT('Ctrl Pts',(-23.0862746896369,-0.5,-3.8)) ;
#23073 = CARTESIAN_POINT('Ctrl Pts',(-22.9137253103631,-0.5,-3.8)) ;
#23074 = CARTESIAN_POINT('Ctrl Pts',(-22.8258541681822,-0.508725003703048,
-3.79288517120475)) ;
#23075 = CARTESIAN_POINT('Ctrl Pts',(-22.6537071359882,-0.543895251562522,
-3.76450988863227)) ;
#23076 = CARTESIAN_POINT('Ctrl Pts',(-22.5694255964999,-0.57032476000931,
-3.74326420954647)) ;
#23077 = CARTESIAN_POINT('Ctrl Pts',(-22.3305352921443,-0.672259420621292,
-3.66289157340511)) ;
#23078 = CARTESIAN_POINT('Ctrl Pts',(-22.1900504239759,-0.771471944939062,
-3.58629392075118)) ;
#23079 = CARTESIAN_POINT('Ctrl Pts',(-21.9675840369442,-0.993938331970815,
-3.43013719509727)) ;
#23080 = CARTESIAN_POINT('Ctrl Pts',(-21.8704353089629,-1.13437448692638,
-3.33760910141692)) ;
#23081 = CARTESIAN_POINT('Ctrl Pts',(-21.7704660290006,-1.36931491352917,
-3.22506776421433)) ;
#23082 = CARTESIAN_POINT('Ctrl Pts',(-21.7444789059789,-1.45178122786162,
-3.19222623476834)) ;
#23083 = CARTESIAN_POINT('Ctrl Pts',(-21.7092429454133,-1.62241691789815,
-3.14593464346712)) ;
#23084 = CARTESIAN_POINT('Ctrl Pts',(-21.7,-1.71065613303991,-3.13273790530888)) ;
#23085 = CARTESIAN_POINT('Ctrl Pts',(-21.7,-1.8,-3.13273790530888)) ;
#23086 = CARTESIAN_POINT('Origin',(-23.,0.85,-2.2)) ;
#23087 = CARTESIAN_POINT('',(-23.6,0.4,-2.2)) ;
#23088 = CARTESIAN_POINT('Origin',(-23.,0.4,-2.2)) ;
#23089 = CARTESIAN_POINT('',(-23.6,1.2,-2.2)) ;
#23090 = CARTESIAN_POINT('',(-23.6,0.85,-2.2)) ;
#23091 = CARTESIAN_POINT('Origin',(-23.,1.2,-2.2)) ;
#23092 = CARTESIAN_POINT('Origin',(-23.,-4.45,-2.2)) ;
#23093 = CARTESIAN_POINT('',(-23.6,-4.8,-2.2)) ;
#23094 = CARTESIAN_POINT('Origin',(-23.,-4.8,-2.2)) ;
#23095 = CARTESIAN_POINT('',(-23.6,-4.,-2.2)) ;
#23096 = CARTESIAN_POINT('',(-23.6,-4.45,-2.2)) ;
#23097 = CARTESIAN_POINT('Origin',(-23.,-4.,-2.2)) ;
#23098 = CARTESIAN_POINT('Origin',(-23.,-1.8,-2.2)) ;
#23099 = CARTESIAN_POINT('',(-24.6,-4.,-2.2)) ;
#23100 = CARTESIAN_POINT('Origin',(-23.,-4.,-2.2)) ;
#23101 = CARTESIAN_POINT('',(-24.6,0.4,-2.2)) ;
#23102 = CARTESIAN_POINT('',(-24.6,-1.8,-2.2)) ;
#23103 = CARTESIAN_POINT('Origin',(-23.,0.4,-2.2)) ;
#23104 = CARTESIAN_POINT('',(-21.9416994755742,-3.2560219778561,-1.)) ;
#23105 = CARTESIAN_POINT('Ctrl Pts',(-21.9416994755742,-3.2560219778561,-1.)) ;
#23106 = CARTESIAN_POINT('Ctrl Pts',(-21.9887809898529,-3.29024288386558,
-0.958478007290045)) ;
#23107 = CARTESIAN_POINT('Ctrl Pts',(-22.0397004336828,-3.32373989107144,
-0.918526128699895)) ;
#23108 = CARTESIAN_POINT('Ctrl Pts',(-22.1778690387736,-3.40421498216876,
-0.823614470242593)) ;
#23109 = CARTESIAN_POINT('Ctrl Pts',(-22.2699364549541,-3.44861974206838,
-0.772284437575066)) ;
#23110 = CARTESIAN_POINT('Ctrl Pts',(-22.4658004734772,-3.522083283395,-0.688049104156577)) ;
#23111 = CARTESIAN_POINT('Ctrl Pts',(-22.5698376966291,-3.55120288441554,
-0.655067419610661)) ;
#23112 = CARTESIAN_POINT('Ctrl Pts',(-22.7831124317021,-3.59017064340857,
-0.611033018569699)) ;
#23113 = CARTESIAN_POINT('Ctrl Pts',(-22.8923574449082,-3.6,-0.6)) ;
#23114 = CARTESIAN_POINT('Ctrl Pts',(-23.1076425550918,-3.6,-0.6)) ;
#23115 = CARTESIAN_POINT('Ctrl Pts',(-23.2168875682979,-3.59017064340857,
-0.611033018569699)) ;
#23116 = CARTESIAN_POINT('Ctrl Pts',(-23.4301623033709,-3.55120288441554,
-0.655067419610661)) ;
#23117 = CARTESIAN_POINT('Ctrl Pts',(-23.5341995265228,-3.522083283395,-0.688049104156577)) ;
#23118 = CARTESIAN_POINT('Ctrl Pts',(-23.7300635450459,-3.44861974206838,
-0.772284437575065)) ;
#23119 = CARTESIAN_POINT('Ctrl Pts',(-23.8221309612264,-3.40421498216876,
-0.823614470242593)) ;
#23120 = CARTESIAN_POINT('Ctrl Pts',(-23.9602995663172,-3.32373989107144,
-0.918526128699897)) ;
#23121 = CARTESIAN_POINT('Ctrl Pts',(-24.0112190101471,-3.29024288386558,
-0.958478007290042)) ;
#23122 = CARTESIAN_POINT('Ctrl Pts',(-24.0583005244258,-3.2560219778561,-1.)) ;
#23123 = CARTESIAN_POINT('',(-21.9416994755742,-1.8,-1.)) ;
#23124 = CARTESIAN_POINT('Ctrl Pts',(-24.0583005244258,-0.343978022143899,
-1.)) ;
#23125 = CARTESIAN_POINT('Ctrl Pts',(-24.0112190101471,-0.309757116134422,
-0.958478007290048)) ;
#23126 = CARTESIAN_POINT('Ctrl Pts',(-23.9602995663172,-0.276260108928558,
-0.918526128699897)) ;
#23127 = CARTESIAN_POINT('Ctrl Pts',(-23.8221309612264,-0.195785017831241,
-0.823614470242595)) ;
#23128 = CARTESIAN_POINT('Ctrl Pts',(-23.7300635450459,-0.151380257931619,
-0.772284437575069)) ;
#23129 = CARTESIAN_POINT('Ctrl Pts',(-23.5341995265228,-0.0779167166050007,
-0.688049104156581)) ;
#23130 = CARTESIAN_POINT('Ctrl Pts',(-23.4301623033709,-0.0487971155844649,
-0.655067419610662)) ;
#23131 = CARTESIAN_POINT('Ctrl Pts',(-23.2168875682979,-0.00982935659143309,
-0.611033018569699)) ;
#23132 = CARTESIAN_POINT('Ctrl Pts',(-23.1076425550918,0.,-0.6)) ;
#23133 = CARTESIAN_POINT('Ctrl Pts',(-22.8923574449082,0.,-0.6)) ;
#23134 = CARTESIAN_POINT('Ctrl Pts',(-22.7831124317021,-0.00982935659143327,
-0.611033018569699)) ;
#23135 = CARTESIAN_POINT('Ctrl Pts',(-22.5698376966291,-0.048797115584464,
-0.655067419610661)) ;
#23136 = CARTESIAN_POINT('Ctrl Pts',(-22.4658004734772,-0.0779167166049992,
-0.688049104156577)) ;
#23137 = CARTESIAN_POINT('Ctrl Pts',(-22.2699364549541,-0.151380257931616,
-0.772284437575065)) ;
#23138 = CARTESIAN_POINT('Ctrl Pts',(-22.1778690387736,-0.195785017831238,
-0.823614470242593)) ;
#23139 = CARTESIAN_POINT('Ctrl Pts',(-22.0397004336828,-0.276260108928556,
-0.918526128699896)) ;
#23140 = CARTESIAN_POINT('Ctrl Pts',(-21.9887809898529,-0.309757116134418,
-0.958478007290042)) ;
#23141 = CARTESIAN_POINT('Ctrl Pts',(-21.9416994755742,-0.343978022143895,
-0.999999999999998)) ;
#23142 = CARTESIAN_POINT('Origin',(-23.,-4.,-2.2)) ;
#23143 = CARTESIAN_POINT('Origin',(-23.,0.4,-2.2)) ;
#23144 = CARTESIAN_POINT('Origin',(-23.,-1.8,-1.)) ;
#23145 = CARTESIAN_POINT('Origin',(-23.,-1.8,-1.)) ;
#23146 = CARTESIAN_POINT('Origin',(-23.,-1.8,-0.45)) ;
#23147 = CARTESIAN_POINT('',(-24.8,-1.8,0.)) ;
#23148 = CARTESIAN_POINT('',(-24.8,-1.8,-0.45)) ;
#23149 = CARTESIAN_POINT('Origin',(-23.,-1.8,0.)) ;
#23150 = CARTESIAN_POINT('Origin',(-23.,-1.8,0.)) ;
#23151 = CARTESIAN_POINT('',(-20.,-4.8,0.)) ;
#23152 = CARTESIAN_POINT('',(-20.,1.2,0.)) ;
#23153 = CARTESIAN_POINT('',(-20.,-1.8,0.)) ;
#23154 = CARTESIAN_POINT('',(-26.,1.2,0.)) ;
#23155 = CARTESIAN_POINT('',(-23.,1.2,0.)) ;
#23156 = CARTESIAN_POINT('',(-26.,-4.8,0.)) ;
#23157 = CARTESIAN_POINT('',(-26.,-1.8,0.)) ;
#23158 = CARTESIAN_POINT('',(-23.,-4.8,0.)) ;
#23159 = CARTESIAN_POINT('Origin',(-23.,-1.8,-4.5)) ;
#23160 = CARTESIAN_POINT('',(-20.,1.2,-4.5)) ;
#23161 = CARTESIAN_POINT('',(-20.,-4.8,-4.5)) ;
#23162 = CARTESIAN_POINT('',(-20.,-1.8,-4.5)) ;
#23163 = CARTESIAN_POINT('',(-26.,-4.8,-4.5)) ;
#23164 = CARTESIAN_POINT('',(-23.,-4.8,-4.5)) ;
#23165 = CARTESIAN_POINT('',(-26.,1.2,-4.5)) ;
#23166 = CARTESIAN_POINT('',(-26.,-1.8,-4.5)) ;
#23167 = CARTESIAN_POINT('',(-23.,1.2,-4.5)) ;
#23168 = CARTESIAN_POINT('Origin',(-23.,-4.8,-2.25)) ;
#23169 = CARTESIAN_POINT('',(-26.,-4.8,-2.25)) ;
#23170 = CARTESIAN_POINT('',(-20.,-4.8,-2.25)) ;
#23171 = CARTESIAN_POINT('Origin',(-26.,-1.8,-2.25)) ;
#23172 = CARTESIAN_POINT('',(-26.,1.2,-2.25)) ;
#23173 = CARTESIAN_POINT('Origin',(-23.,1.2,-2.25)) ;
#23174 = CARTESIAN_POINT('',(-20.,1.2,-2.25)) ;
#23175 = CARTESIAN_POINT('Origin',(-20.,-1.8,-2.25)) ;
#23176 = CARTESIAN_POINT('',(0.,0.,0.)) ;
#23177 = CARTESIAN_POINT('Origin',(-23.,-1.8,-2.2)) ;
#23178 = CARTESIAN_POINT('',(-23.4,-3.8,-2.2)) ;
#23179 = CARTESIAN_POINT('Origin',(-23.,-3.8,-2.2)) ;
#23180 = CARTESIAN_POINT('',(-23.4,0.2,-2.2)) ;
#23181 = CARTESIAN_POINT('',(-23.4,-1.8,-2.2)) ;
#23182 = CARTESIAN_POINT('Origin',(-23.,0.2,-2.2)) ;
#23183 = CARTESIAN_POINT('Origin',(-21.9393398282202,-1.8,-3.26066017177982)) ;
#23184 = CARTESIAN_POINT('',(-22.1716217408478,-3.8,-3.45051567753628)) ;
#23185 = CARTESIAN_POINT('',(-21.7494843224637,-3.8,-3.02837825915217)) ;
#23186 = CARTESIAN_POINT('Origin',(-21.9393398282202,-3.8,-3.26066017177982)) ;
#23187 = CARTESIAN_POINT('',(-22.1716217408478,0.2,-3.45051567753628)) ;
#23188 = CARTESIAN_POINT('',(-22.1716217408478,-1.8,-3.45051567753628)) ;
#23189 = CARTESIAN_POINT('',(-21.7494843224637,0.2,-3.02837825915217)) ;
#23190 = CARTESIAN_POINT('Origin',(-21.9393398282202,0.2,-3.26066017177982)) ;
#23191 = CARTESIAN_POINT('',(-21.7494843224637,-1.8,-3.02837825915217)) ;
#23192 = CARTESIAN_POINT('Origin',(-23.,0.2,-2.2)) ;
#23193 = CARTESIAN_POINT('',(-22.701503768868,0.2,-3.67)) ;
#23194 = CARTESIAN_POINT('Origin',(-23.,0.2,-2.2)) ;
#23195 = CARTESIAN_POINT('',(-23.298496231132,0.2,-3.67)) ;
#23196 = CARTESIAN_POINT('Origin',(-23.,0.2,-3.7)) ;
#23197 = CARTESIAN_POINT('',(-23.8283782591522,0.2,-3.45051567753628)) ;
#23198 = CARTESIAN_POINT('Origin',(-23.,0.2,-2.2)) ;
#23199 = CARTESIAN_POINT('',(-24.2505156775363,0.2,-3.02837825915217)) ;
#23200 = CARTESIAN_POINT('Origin',(-24.0606601717798,0.2,-3.26066017177982)) ;
#23201 = CARTESIAN_POINT('',(-24.47,0.2,-2.49849623113198)) ;
#23202 = CARTESIAN_POINT('Origin',(-23.,0.2,-2.2)) ;
#23203 = CARTESIAN_POINT('',(-24.47,0.2,-1.90150376886801)) ;
#23204 = CARTESIAN_POINT('Origin',(-24.5,0.2,-2.2)) ;
#23205 = CARTESIAN_POINT('',(-24.2505156775363,0.2,-1.37162174084783)) ;
#23206 = CARTESIAN_POINT('Origin',(-23.,0.2,-2.2)) ;
#23207 = CARTESIAN_POINT('',(-23.8283782591522,0.2,-0.949484322463722)) ;
#23208 = CARTESIAN_POINT('Origin',(-24.0606601717798,0.2,-1.13933982822018)) ;
#23209 = CARTESIAN_POINT('',(-23.298496231132,0.2,-0.73)) ;
#23210 = CARTESIAN_POINT('Origin',(-23.,0.2,-2.2)) ;
#23211 = CARTESIAN_POINT('',(-22.701503768868,0.2,-0.73)) ;
#23212 = CARTESIAN_POINT('Origin',(-23.,0.2,-0.7)) ;
#23213 = CARTESIAN_POINT('',(-22.1716217408478,0.2,-0.94948432246372)) ;
#23214 = CARTESIAN_POINT('Origin',(-23.,0.2,-2.2)) ;
#23215 = CARTESIAN_POINT('',(-21.7494843224637,0.2,-1.37162174084783)) ;
#23216 = CARTESIAN_POINT('Origin',(-21.9393398282202,0.2,-1.13933982822018)) ;
#23217 = CARTESIAN_POINT('',(-21.53,0.2,-1.90150376886802)) ;
#23218 = CARTESIAN_POINT('Origin',(-23.,0.2,-2.2)) ;
#23219 = CARTESIAN_POINT('',(-21.53,0.2,-2.49849623113198)) ;
#23220 = CARTESIAN_POINT('Origin',(-21.5,0.2,-2.2)) ;
#23221 = CARTESIAN_POINT('Origin',(-23.,0.2,-2.2)) ;
#23222 = CARTESIAN_POINT('Origin',(-23.,-1.8,-2.2)) ;
#23223 = CARTESIAN_POINT('',(-22.701503768868,-3.8,-3.67)) ;
#23224 = CARTESIAN_POINT('Origin',(-23.,-3.8,-2.2)) ;
#23225 = CARTESIAN_POINT('',(-22.701503768868,-1.8,-3.67)) ;
#23226 = CARTESIAN_POINT('Origin',(-23.,-1.8,-3.7)) ;
#23227 = CARTESIAN_POINT('',(-23.298496231132,-3.8,-3.67)) ;
#23228 = CARTESIAN_POINT('Origin',(-23.,-3.8,-3.7)) ;
#23229 = CARTESIAN_POINT('',(-23.298496231132,-1.8,-3.67)) ;
#23230 = CARTESIAN_POINT('Origin',(-23.,-1.8,-2.2)) ;
#23231 = CARTESIAN_POINT('',(-23.8283782591522,-3.8,-3.45051567753628)) ;
#23232 = CARTESIAN_POINT('Origin',(-23.,-3.8,-2.2)) ;
#23233 = CARTESIAN_POINT('',(-23.8283782591522,-1.8,-3.45051567753628)) ;
#23234 = CARTESIAN_POINT('Origin',(-24.0606601717798,-1.8,-3.26066017177982)) ;
#23235 = CARTESIAN_POINT('',(-24.2505156775363,-3.8,-3.02837825915217)) ;
#23236 = CARTESIAN_POINT('Origin',(-24.0606601717798,-3.8,-3.26066017177982)) ;
#23237 = CARTESIAN_POINT('',(-24.2505156775363,-1.8,-3.02837825915217)) ;
#23238 = CARTESIAN_POINT('Origin',(-23.,-1.8,-2.2)) ;
#23239 = CARTESIAN_POINT('',(-24.47,-3.8,-2.49849623113198)) ;
#23240 = CARTESIAN_POINT('Origin',(-23.,-3.8,-2.2)) ;
#23241 = CARTESIAN_POINT('',(-24.47,-1.8,-2.49849623113199)) ;
#23242 = CARTESIAN_POINT('Origin',(-24.5,-1.8,-2.2)) ;
#23243 = CARTESIAN_POINT('',(-24.47,-3.8,-1.90150376886801)) ;
#23244 = CARTESIAN_POINT('Origin',(-24.5,-3.8,-2.2)) ;
#23245 = CARTESIAN_POINT('',(-24.47,-1.8,-1.90150376886801)) ;
#23246 = CARTESIAN_POINT('Origin',(-23.,-1.8,-2.2)) ;
#23247 = CARTESIAN_POINT('',(-24.2505156775363,-3.8,-1.37162174084783)) ;
#23248 = CARTESIAN_POINT('Origin',(-23.,-3.8,-2.2)) ;
#23249 = CARTESIAN_POINT('',(-24.2505156775363,-1.8,-1.37162174084783)) ;
#23250 = CARTESIAN_POINT('Origin',(-24.0606601717798,-1.8,-1.13933982822018)) ;
#23251 = CARTESIAN_POINT('',(-23.8283782591522,-3.8,-0.949484322463722)) ;
#23252 = CARTESIAN_POINT('Origin',(-24.0606601717798,-3.8,-1.13933982822018)) ;
#23253 = CARTESIAN_POINT('',(-23.8283782591522,-1.8,-0.949484322463721)) ;
#23254 = CARTESIAN_POINT('Origin',(-23.,-1.8,-2.2)) ;
#23255 = CARTESIAN_POINT('',(-23.298496231132,-3.8,-0.73)) ;
#23256 = CARTESIAN_POINT('Origin',(-23.,-3.8,-2.2)) ;
#23257 = CARTESIAN_POINT('',(-23.298496231132,-1.8,-0.73)) ;
#23258 = CARTESIAN_POINT('Origin',(-23.,-1.8,-0.7)) ;
#23259 = CARTESIAN_POINT('',(-22.701503768868,-3.8,-0.73)) ;
#23260 = CARTESIAN_POINT('Origin',(-23.,-3.8,-0.7)) ;
#23261 = CARTESIAN_POINT('',(-22.701503768868,-1.8,-0.73)) ;
#23262 = CARTESIAN_POINT('Origin',(-23.,-1.8,-2.2)) ;
#23263 = CARTESIAN_POINT('',(-22.1716217408478,-3.8,-0.94948432246372)) ;
#23264 = CARTESIAN_POINT('Origin',(-23.,-3.8,-2.2)) ;
#23265 = CARTESIAN_POINT('',(-22.1716217408478,-1.8,-0.94948432246372)) ;
#23266 = CARTESIAN_POINT('Origin',(-21.9393398282202,-1.8,-1.13933982822018)) ;
#23267 = CARTESIAN_POINT('',(-21.7494843224637,-3.8,-1.37162174084783)) ;
#23268 = CARTESIAN_POINT('Origin',(-21.9393398282202,-3.8,-1.13933982822018)) ;
#23269 = CARTESIAN_POINT('',(-21.7494843224637,-1.8,-1.37162174084783)) ;
#23270 = CARTESIAN_POINT('Origin',(-23.,-1.8,-2.2)) ;
#23271 = CARTESIAN_POINT('',(-21.53,-3.8,-1.90150376886802)) ;
#23272 = CARTESIAN_POINT('Origin',(-23.,-3.8,-2.2)) ;
#23273 = CARTESIAN_POINT('',(-21.53,-1.8,-1.90150376886801)) ;
#23274 = CARTESIAN_POINT('Origin',(-21.5,-1.8,-2.2)) ;
#23275 = CARTESIAN_POINT('',(-21.53,-3.8,-2.49849623113198)) ;
#23276 = CARTESIAN_POINT('Origin',(-21.5,-3.8,-2.2)) ;
#23277 = CARTESIAN_POINT('',(-21.53,-1.8,-2.49849623113199)) ;
#23278 = CARTESIAN_POINT('Origin',(-23.,-3.8,-2.2)) ;
#23279 = CARTESIAN_POINT('Origin',(-23.,-3.8,-2.2)) ;
#23280 = CARTESIAN_POINT('Origin',(-23.,-1.8,-2.2)) ;
#23281 = CARTESIAN_POINT('',(0.,0.,0.)) ;
#23282 = CARTESIAN_POINT('Origin',(-23.,-1.,-2.2)) ;
#23283 = CARTESIAN_POINT('',(-23.4,3.,-2.2)) ;
#23284 = CARTESIAN_POINT('Origin',(-23.,3.,-2.2)) ;
#23285 = CARTESIAN_POINT('',(-23.4,-5.,-2.2)) ;
#23286 = CARTESIAN_POINT('',(-23.4,-1.,-2.2)) ;
#23287 = CARTESIAN_POINT('Origin',(-23.,-5.,-2.2)) ;
#23288 = CARTESIAN_POINT('Origin',(-23.,-5.,-2.2)) ;
#23289 = CARTESIAN_POINT('Origin',(-23.,3.,-2.2)) ;
#23290 = CARTESIAN_POINT('',(0.,0.,0.)) ;
#23291 = CARTESIAN_POINT('Origin',(-23.,-4.4,-2.2)) ;
#23292 = CARTESIAN_POINT('',(-23.4,-4.8,-2.2)) ;
#23293 = CARTESIAN_POINT('Origin',(-23.,-4.8,-2.2)) ;
#23294 = CARTESIAN_POINT('',(-23.4,-4.,-2.2)) ;
#23295 = CARTESIAN_POINT('',(-23.4,-4.4,-2.2)) ;
#23296 = CARTESIAN_POINT('Origin',(-23.,-4.,-2.2)) ;
#23297 = CARTESIAN_POINT('Origin',(-23.,-4.4,-2.2)) ;
#23298 = CARTESIAN_POINT('',(-23.6,-4.,-2.2)) ;
#23299 = CARTESIAN_POINT('Origin',(-23.,-4.,-2.2)) ;
#23300 = CARTESIAN_POINT('',(-23.6,-4.8,-2.2)) ;
#23301 = CARTESIAN_POINT('',(-23.6,-4.4,-2.2)) ;
#23302 = CARTESIAN_POINT('Origin',(-23.,-4.8,-2.2)) ;
#23303 = CARTESIAN_POINT('Origin',(-23.,-4.8,-2.2)) ;
#23304 = CARTESIAN_POINT('Origin',(-23.,-4.,-2.2)) ;
#23305 = CARTESIAN_POINT('',(0.,0.,0.)) ;
#23306 = CARTESIAN_POINT('Origin',(-23.,2.1,-2.2)) ;
#23307 = CARTESIAN_POINT('',(-23.4,1.6,-2.2)) ;
#23308 = CARTESIAN_POINT('Origin',(-23.,1.6,-2.2)) ;
#23309 = CARTESIAN_POINT('',(-23.4,2.6,-2.2)) ;
#23310 = CARTESIAN_POINT('',(-23.4,2.1,-2.2)) ;
#23311 = CARTESIAN_POINT('Origin',(-23.,2.6,-2.2)) ;
#23312 = CARTESIAN_POINT('Origin',(-23.,2.1,-2.2)) ;
#23313 = CARTESIAN_POINT('',(-23.8,2.,-2.2)) ;
#23314 = CARTESIAN_POINT('Origin',(-23.,2.,-2.2)) ;
#23315 = CARTESIAN_POINT('',(-23.8,1.6,-2.2)) ;
#23316 = CARTESIAN_POINT('',(-23.8,2.1,-2.2)) ;
#23317 = CARTESIAN_POINT('Origin',(-23.,1.6,-2.2)) ;
#23318 = CARTESIAN_POINT('Origin',(-23.,1.6,-2.2)) ;
#23319 = CARTESIAN_POINT('Origin',(-21.6651219592813,2.05,-3.16984566628258)) ;
#23320 = CARTESIAN_POINT('',(-21.9148668248458,2.05,-3.23560899579898)) ;
#23321 = CARTESIAN_POINT('',(-21.6797527239288,2.05,-2.912002198049)) ;
#23322 = CARTESIAN_POINT('Origin',(-23.,2.05,-2.2)) ;
#23323 = CARTESIAN_POINT('',(-21.6208756108648,2.05,-3.44920611561607)) ;
#23324 = CARTESIAN_POINT('',(-21.7826790097398,2.05,-3.33164906515757)) ;
#23325 = CARTESIAN_POINT('',(-21.3857615099479,2.05,-3.12559931786609)) ;
#23326 = CARTESIAN_POINT('',(-21.5033185604063,2.05,-3.28740271674108)) ;
#23327 = CARTESIAN_POINT('',(-21.5475649088228,2.05,-3.00804226740759)) ;
#23328 = CARTESIAN_POINT('Origin',(-21.7826790097398,2.3,-3.33164906515757)) ;
#23329 = CARTESIAN_POINT('',(-21.9148668248458,2.55,-3.23560899579898)) ;
#23330 = CARTESIAN_POINT('',(-21.9148668248458,2.3,-3.23560899579898)) ;
#23331 = CARTESIAN_POINT('',(-21.6208756108648,2.55,-3.44920611561607)) ;
#23332 = CARTESIAN_POINT('',(-21.7826790097398,2.55,-3.33164906515757)) ;
#23333 = CARTESIAN_POINT('',(-21.6208756108648,2.3,-3.44920611561607)) ;
#23334 = CARTESIAN_POINT('Origin',(-21.5475649088228,2.3,-3.00804226740759)) ;
#23335 = CARTESIAN_POINT('',(-21.6797527239288,2.55,-2.912002198049)) ;
#23336 = CARTESIAN_POINT('',(-21.6797527239288,2.3,-2.912002198049)) ;
#23337 = CARTESIAN_POINT('',(-21.3857615099479,2.55,-3.12559931786609)) ;
#23338 = CARTESIAN_POINT('',(-21.3857615099479,2.3,-3.12559931786609)) ;
#23339 = CARTESIAN_POINT('',(-21.5475649088228,2.55,-3.00804226740759)) ;
#23340 = CARTESIAN_POINT('Origin',(-21.6651219592813,2.55,-3.16984566628258)) ;
#23341 = CARTESIAN_POINT('Origin',(-23.,2.55,-2.2)) ;
#23342 = CARTESIAN_POINT('',(-21.5033185604063,2.55,-3.28740271674108)) ;
#23343 = CARTESIAN_POINT('Origin',(-21.5033185604063,2.3,-3.28740271674108)) ;
#23344 = CARTESIAN_POINT('Origin',(-22.4901219592813,2.05,-3.769243251887)) ;
#23345 = CARTESIAN_POINT('',(-22.7308245150123,2.05,-3.67565055425789)) ;
#23346 = CARTESIAN_POINT('',(-22.3504019084942,2.05,-3.55204375650791)) ;
#23347 = CARTESIAN_POINT('Origin',(-23.,2.05,-2.2)) ;
#23348 = CARTESIAN_POINT('',(-22.6185298636654,2.05,-4.02125795402102)) ;
#23349 = CARTESIAN_POINT('',(-22.6803332625404,2.05,-3.83104665076199)) ;
#23350 = CARTESIAN_POINT('',(-22.2381072571473,2.05,-3.89765115627104)) ;
#23351 = CARTESIAN_POINT('',(-22.4283185604063,2.05,-3.95945455514603)) ;
#23352 = CARTESIAN_POINT('',(-22.2999106560223,2.05,-3.70743985301201)) ;
#23353 = CARTESIAN_POINT('Origin',(-22.6803332625404,2.3,-3.83104665076199)) ;
#23354 = CARTESIAN_POINT('',(-22.7308245150123,2.55,-3.67565055425789)) ;
#23355 = CARTESIAN_POINT('',(-22.7308245150123,2.3,-3.67565055425789)) ;
#23356 = CARTESIAN_POINT('',(-22.6185298636654,2.55,-4.02125795402102)) ;
#23357 = CARTESIAN_POINT('',(-22.6803332625404,2.55,-3.83104665076199)) ;
#23358 = CARTESIAN_POINT('',(-22.6185298636654,2.3,-4.02125795402102)) ;
#23359 = CARTESIAN_POINT('Origin',(-22.2999106560223,2.3,-3.70743985301201)) ;
#23360 = CARTESIAN_POINT('',(-22.3504019084942,2.55,-3.55204375650791)) ;
#23361 = CARTESIAN_POINT('',(-22.3504019084942,2.3,-3.55204375650791)) ;
#23362 = CARTESIAN_POINT('',(-22.2381072571473,2.55,-3.89765115627104)) ;
#23363 = CARTESIAN_POINT('',(-22.2381072571473,2.3,-3.89765115627104)) ;
#23364 = CARTESIAN_POINT('',(-22.2999106560223,2.55,-3.70743985301201)) ;
#23365 = CARTESIAN_POINT('Origin',(-22.4901219592813,2.55,-3.769243251887)) ;
#23366 = CARTESIAN_POINT('Origin',(-23.,2.55,-2.2)) ;
#23367 = CARTESIAN_POINT('',(-22.4283185604063,2.55,-3.95945455514603)) ;
#23368 = CARTESIAN_POINT('Origin',(-22.4283185604063,2.3,-3.95945455514603)) ;
#23369 = CARTESIAN_POINT('Origin',(-23.5098780407187,2.05,-3.769243251887)) ;
#23370 = CARTESIAN_POINT('',(-23.6495980915058,2.05,-3.55204375650791)) ;
#23371 = CARTESIAN_POINT('',(-23.2691754849877,2.05,-3.67565055425789)) ;
#23372 = CARTESIAN_POINT('Origin',(-23.,2.05,-2.2)) ;
#23373 = CARTESIAN_POINT('',(-23.7618927428527,2.05,-3.89765115627104)) ;
#23374 = CARTESIAN_POINT('',(-23.7000893439777,2.05,-3.70743985301201)) ;
#23375 = CARTESIAN_POINT('',(-23.3814701363346,2.05,-4.02125795402102)) ;
#23376 = CARTESIAN_POINT('',(-23.5716814395937,2.05,-3.95945455514603)) ;
#23377 = CARTESIAN_POINT('',(-23.3196667374596,2.05,-3.83104665076199)) ;
#23378 = CARTESIAN_POINT('Origin',(-23.7000893439777,2.3,-3.70743985301201)) ;
#23379 = CARTESIAN_POINT('',(-23.6495980915058,2.55,-3.55204375650791)) ;
#23380 = CARTESIAN_POINT('',(-23.6495980915058,2.3,-3.55204375650791)) ;
#23381 = CARTESIAN_POINT('',(-23.7618927428527,2.55,-3.89765115627104)) ;
#23382 = CARTESIAN_POINT('',(-23.7000893439777,2.55,-3.70743985301201)) ;
#23383 = CARTESIAN_POINT('',(-23.7618927428527,2.3,-3.89765115627104)) ;
#23384 = CARTESIAN_POINT('Origin',(-23.3196667374596,2.3,-3.83104665076199)) ;
#23385 = CARTESIAN_POINT('',(-23.2691754849877,2.55,-3.67565055425789)) ;
#23386 = CARTESIAN_POINT('',(-23.2691754849877,2.3,-3.67565055425789)) ;
#23387 = CARTESIAN_POINT('',(-23.3814701363346,2.55,-4.02125795402102)) ;
#23388 = CARTESIAN_POINT('',(-23.3814701363346,2.3,-4.02125795402102)) ;
#23389 = CARTESIAN_POINT('',(-23.3196667374596,2.55,-3.83104665076199)) ;
#23390 = CARTESIAN_POINT('Origin',(-23.5098780407187,2.55,-3.769243251887)) ;
#23391 = CARTESIAN_POINT('Origin',(-23.,2.55,-2.2)) ;
#23392 = CARTESIAN_POINT('',(-23.5716814395937,2.55,-3.95945455514603)) ;
#23393 = CARTESIAN_POINT('Origin',(-23.5716814395937,2.3,-3.95945455514603)) ;
#23394 = CARTESIAN_POINT('Origin',(-24.3348780407187,2.05,-3.16984566628258)) ;
#23395 = CARTESIAN_POINT('',(-24.3202472760712,2.05,-2.912002198049)) ;
#23396 = CARTESIAN_POINT('',(-24.0851331751542,2.05,-3.23560899579897)) ;
#23397 = CARTESIAN_POINT('Origin',(-23.,2.05,-2.2)) ;
#23398 = CARTESIAN_POINT('',(-24.6142384900521,2.05,-3.12559931786609)) ;
#23399 = CARTESIAN_POINT('',(-24.4524350911772,2.05,-3.00804226740759)) ;
#23400 = CARTESIAN_POINT('',(-24.3791243891352,2.05,-3.44920611561606)) ;
#23401 = CARTESIAN_POINT('',(-24.4966814395937,2.05,-3.28740271674108)) ;
#23402 = CARTESIAN_POINT('',(-24.2173209902602,2.05,-3.33164906515757)) ;
#23403 = CARTESIAN_POINT('Origin',(-24.4524350911772,2.3,-3.00804226740759)) ;
#23404 = CARTESIAN_POINT('',(-24.3202472760712,2.55,-2.912002198049)) ;
#23405 = CARTESIAN_POINT('',(-24.3202472760712,2.3,-2.912002198049)) ;
#23406 = CARTESIAN_POINT('',(-24.6142384900521,2.55,-3.12559931786609)) ;
#23407 = CARTESIAN_POINT('',(-24.4524350911772,2.55,-3.00804226740759)) ;
#23408 = CARTESIAN_POINT('',(-24.6142384900521,2.3,-3.12559931786609)) ;
#23409 = CARTESIAN_POINT('Origin',(-24.2173209902602,2.3,-3.33164906515757)) ;
#23410 = CARTESIAN_POINT('',(-24.0851331751542,2.55,-3.23560899579897)) ;
#23411 = CARTESIAN_POINT('',(-24.0851331751542,2.3,-3.23560899579897)) ;
#23412 = CARTESIAN_POINT('',(-24.3791243891352,2.55,-3.44920611561606)) ;
#23413 = CARTESIAN_POINT('',(-24.3791243891352,2.3,-3.44920611561606)) ;
#23414 = CARTESIAN_POINT('',(-24.2173209902602,2.55,-3.33164906515757)) ;
#23415 = CARTESIAN_POINT('Origin',(-24.3348780407187,2.55,-3.16984566628258)) ;
#23416 = CARTESIAN_POINT('Origin',(-23.,2.55,-2.2)) ;
#23417 = CARTESIAN_POINT('',(-24.4966814395937,2.55,-3.28740271674108)) ;
#23418 = CARTESIAN_POINT('Origin',(-24.4966814395937,2.3,-3.28740271674108)) ;
#23419 = CARTESIAN_POINT('Origin',(-24.65,2.05,-2.2)) ;
#23420 = CARTESIAN_POINT('',(-24.4866068747319,2.05,-2.)) ;
#23421 = CARTESIAN_POINT('',(-24.5,2.05,-2.2)) ;
#23422 = CARTESIAN_POINT('Origin',(-23.,2.05,-2.2)) ;
#23423 = CARTESIAN_POINT('',(-24.85,2.05,-2.)) ;
#23424 = CARTESIAN_POINT('',(-24.65,2.05,-2.)) ;
#23425 = CARTESIAN_POINT('',(-24.85,2.05,-2.4)) ;
#23426 = CARTESIAN_POINT('',(-24.85,2.05,-2.2)) ;
#23427 = CARTESIAN_POINT('',(-24.4866068747319,2.05,-2.4)) ;
#23428 = CARTESIAN_POINT('',(-24.65,2.05,-2.4)) ;
#23429 = CARTESIAN_POINT('Origin',(-23.,2.05,-2.2)) ;
#23430 = CARTESIAN_POINT('Origin',(-24.65,2.3,-2.)) ;
#23431 = CARTESIAN_POINT('',(-24.4866068747319,2.55,-2.)) ;
#23432 = CARTESIAN_POINT('',(-24.4866068747319,2.3,-2.)) ;
#23433 = CARTESIAN_POINT('',(-24.85,2.55,-2.)) ;
#23434 = CARTESIAN_POINT('',(-24.65,2.55,-2.)) ;
#23435 = CARTESIAN_POINT('',(-24.85,2.3,-2.)) ;
#23436 = CARTESIAN_POINT('Origin',(-24.65,2.3,-2.4)) ;
#23437 = CARTESIAN_POINT('',(-24.4866068747319,2.55,-2.4)) ;
#23438 = CARTESIAN_POINT('',(-24.4866068747319,2.3,-2.4)) ;
#23439 = CARTESIAN_POINT('',(-24.85,2.55,-2.4)) ;
#23440 = CARTESIAN_POINT('',(-24.85,2.3,-2.4)) ;
#23441 = CARTESIAN_POINT('',(-24.65,2.55,-2.4)) ;
#23442 = CARTESIAN_POINT('Origin',(-24.65,2.55,-2.2)) ;
#23443 = CARTESIAN_POINT('',(-24.5,2.55,-2.2)) ;
#23444 = CARTESIAN_POINT('Origin',(-23.,2.55,-2.2)) ;
#23445 = CARTESIAN_POINT('',(-24.85,2.55,-2.2)) ;
#23446 = CARTESIAN_POINT('Origin',(-23.,2.55,-2.2)) ;
#23447 = CARTESIAN_POINT('Origin',(-24.85,2.3,-2.2)) ;
#23448 = CARTESIAN_POINT('Origin',(-24.3348780407187,2.05,-1.23015433371742)) ;
#23449 = CARTESIAN_POINT('',(-24.0851331751542,2.05,-1.16439100420103)) ;
#23450 = CARTESIAN_POINT('',(-24.3202472760712,2.05,-1.487997801951)) ;
#23451 = CARTESIAN_POINT('Origin',(-23.,2.05,-2.2)) ;
#23452 = CARTESIAN_POINT('',(-24.3791243891352,2.05,-0.950793884383935)) ;
#23453 = CARTESIAN_POINT('',(-24.2173209902602,2.05,-1.06835093484243)) ;
#23454 = CARTESIAN_POINT('',(-24.6142384900521,2.05,-1.27440068213391)) ;
#23455 = CARTESIAN_POINT('',(-24.4966814395937,2.05,-1.11259728325892)) ;
#23456 = CARTESIAN_POINT('',(-24.4524350911772,2.05,-1.39195773259241)) ;
#23457 = CARTESIAN_POINT('Origin',(-24.2173209902602,2.3,-1.06835093484243)) ;
#23458 = CARTESIAN_POINT('',(-24.0851331751542,2.55,-1.16439100420103)) ;
#23459 = CARTESIAN_POINT('',(-24.0851331751542,2.3,-1.16439100420103)) ;
#23460 = CARTESIAN_POINT('',(-24.3791243891352,2.55,-0.950793884383935)) ;
#23461 = CARTESIAN_POINT('',(-24.2173209902602,2.55,-1.06835093484243)) ;
#23462 = CARTESIAN_POINT('',(-24.3791243891352,2.3,-0.950793884383935)) ;
#23463 = CARTESIAN_POINT('Origin',(-24.4524350911772,2.3,-1.39195773259241)) ;
#23464 = CARTESIAN_POINT('',(-24.3202472760712,2.55,-1.487997801951)) ;
#23465 = CARTESIAN_POINT('',(-24.3202472760712,2.3,-1.487997801951)) ;
#23466 = CARTESIAN_POINT('',(-24.6142384900521,2.55,-1.27440068213391)) ;
#23467 = CARTESIAN_POINT('',(-24.6142384900521,2.3,-1.27440068213391)) ;
#23468 = CARTESIAN_POINT('',(-24.4524350911772,2.55,-1.39195773259241)) ;
#23469 = CARTESIAN_POINT('Origin',(-24.3348780407187,2.55,-1.23015433371742)) ;
#23470 = CARTESIAN_POINT('Origin',(-23.,2.55,-2.2)) ;
#23471 = CARTESIAN_POINT('',(-24.4966814395937,2.55,-1.11259728325892)) ;
#23472 = CARTESIAN_POINT('Origin',(-24.4966814395937,2.3,-1.11259728325892)) ;
#23473 = CARTESIAN_POINT('Origin',(-23.5098780407187,2.05,-0.630756748112997)) ;
#23474 = CARTESIAN_POINT('',(-23.2691754849877,2.05,-0.724349445742112)) ;
#23475 = CARTESIAN_POINT('',(-23.6495980915058,2.05,-0.847956243492091)) ;
#23476 = CARTESIAN_POINT('Origin',(-23.,2.05,-2.2)) ;
#23477 = CARTESIAN_POINT('',(-23.3814701363346,2.05,-0.378742045978976)) ;
#23478 = CARTESIAN_POINT('',(-23.3196667374596,2.05,-0.568953349238007)) ;
#23479 = CARTESIAN_POINT('',(-23.7618927428527,2.05,-0.502348843728955)) ;
#23480 = CARTESIAN_POINT('',(-23.5716814395937,2.05,-0.440545444853966)) ;
#23481 = CARTESIAN_POINT('',(-23.7000893439777,2.05,-0.692560146987986)) ;
#23482 = CARTESIAN_POINT('Origin',(-23.3196667374596,2.3,-0.568953349238007)) ;
#23483 = CARTESIAN_POINT('',(-23.2691754849877,2.55,-0.724349445742112)) ;
#23484 = CARTESIAN_POINT('',(-23.2691754849877,2.3,-0.724349445742112)) ;
#23485 = CARTESIAN_POINT('',(-23.3814701363346,2.55,-0.378742045978976)) ;
#23486 = CARTESIAN_POINT('',(-23.3196667374596,2.55,-0.568953349238007)) ;
#23487 = CARTESIAN_POINT('',(-23.3814701363346,2.3,-0.378742045978976)) ;
#23488 = CARTESIAN_POINT('Origin',(-23.7000893439777,2.3,-0.692560146987986)) ;
#23489 = CARTESIAN_POINT('',(-23.6495980915058,2.55,-0.847956243492091)) ;
#23490 = CARTESIAN_POINT('',(-23.6495980915058,2.3,-0.847956243492091)) ;
#23491 = CARTESIAN_POINT('',(-23.7618927428527,2.55,-0.502348843728955)) ;
#23492 = CARTESIAN_POINT('',(-23.7618927428527,2.3,-0.502348843728955)) ;
#23493 = CARTESIAN_POINT('',(-23.7000893439777,2.55,-0.692560146987986)) ;
#23494 = CARTESIAN_POINT('Origin',(-23.5098780407187,2.55,-0.630756748112997)) ;
#23495 = CARTESIAN_POINT('Origin',(-23.,2.55,-2.2)) ;
#23496 = CARTESIAN_POINT('',(-23.5716814395937,2.55,-0.440545444853966)) ;
#23497 = CARTESIAN_POINT('Origin',(-23.5716814395937,2.3,-0.440545444853966)) ;
#23498 = CARTESIAN_POINT('Origin',(-22.4901219592813,2.05,-0.630756748112997)) ;
#23499 = CARTESIAN_POINT('',(-22.3504019084942,2.05,-0.847956243492089)) ;
#23500 = CARTESIAN_POINT('',(-22.7308245150123,2.05,-0.724349445742111)) ;
#23501 = CARTESIAN_POINT('Origin',(-23.,2.05,-2.2)) ;
#23502 = CARTESIAN_POINT('',(-22.2381072571473,2.05,-0.502348843728955)) ;
#23503 = CARTESIAN_POINT('',(-22.2999106560223,2.05,-0.692560146987986)) ;
#23504 = CARTESIAN_POINT('',(-22.6185298636654,2.05,-0.378742045978977)) ;
#23505 = CARTESIAN_POINT('',(-22.4283185604063,2.05,-0.440545444853966)) ;
#23506 = CARTESIAN_POINT('',(-22.6803332625404,2.05,-0.568953349238007)) ;
#23507 = CARTESIAN_POINT('Origin',(-22.2999106560223,2.3,-0.692560146987986)) ;
#23508 = CARTESIAN_POINT('',(-22.3504019084942,2.55,-0.847956243492089)) ;
#23509 = CARTESIAN_POINT('',(-22.3504019084942,2.3,-0.84795624349209)) ;
#23510 = CARTESIAN_POINT('',(-22.2381072571473,2.55,-0.502348843728955)) ;
#23511 = CARTESIAN_POINT('',(-22.2999106560223,2.55,-0.692560146987986)) ;
#23512 = CARTESIAN_POINT('',(-22.2381072571473,2.3,-0.502348843728955)) ;
#23513 = CARTESIAN_POINT('Origin',(-22.6803332625404,2.3,-0.568953349238007)) ;
#23514 = CARTESIAN_POINT('',(-22.7308245150123,2.55,-0.724349445742111)) ;
#23515 = CARTESIAN_POINT('',(-22.7308245150123,2.3,-0.724349445742111)) ;
#23516 = CARTESIAN_POINT('',(-22.6185298636654,2.55,-0.378742045978977)) ;
#23517 = CARTESIAN_POINT('',(-22.6185298636654,2.3,-0.378742045978977)) ;
#23518 = CARTESIAN_POINT('',(-22.6803332625404,2.55,-0.568953349238007)) ;
#23519 = CARTESIAN_POINT('Origin',(-22.4901219592813,2.55,-0.630756748112997)) ;
#23520 = CARTESIAN_POINT('Origin',(-23.,2.55,-2.2)) ;
#23521 = CARTESIAN_POINT('',(-22.4283185604063,2.55,-0.440545444853966)) ;
#23522 = CARTESIAN_POINT('Origin',(-22.4283185604063,2.3,-0.440545444853966)) ;
#23523 = CARTESIAN_POINT('Origin',(-21.6651219592813,2.05,-1.23015433371742)) ;
#23524 = CARTESIAN_POINT('',(-21.6797527239288,2.05,-1.487997801951)) ;
#23525 = CARTESIAN_POINT('',(-21.9148668248458,2.05,-1.16439100420103)) ;
#23526 = CARTESIAN_POINT('Origin',(-23.,2.05,-2.2)) ;
#23527 = CARTESIAN_POINT('',(-21.3857615099479,2.05,-1.27440068213391)) ;
#23528 = CARTESIAN_POINT('',(-21.5475649088228,2.05,-1.39195773259241)) ;
#23529 = CARTESIAN_POINT('',(-21.6208756108648,2.05,-0.950793884383935)) ;
#23530 = CARTESIAN_POINT('',(-21.5033185604063,2.05,-1.11259728325892)) ;
#23531 = CARTESIAN_POINT('',(-21.7826790097398,2.05,-1.06835093484243)) ;
#23532 = CARTESIAN_POINT('Origin',(-21.5475649088228,2.3,-1.39195773259241)) ;
#23533 = CARTESIAN_POINT('',(-21.6797527239288,2.55,-1.487997801951)) ;
#23534 = CARTESIAN_POINT('',(-21.6797527239288,2.3,-1.487997801951)) ;
#23535 = CARTESIAN_POINT('',(-21.3857615099479,2.55,-1.27440068213391)) ;
#23536 = CARTESIAN_POINT('',(-21.5475649088228,2.55,-1.39195773259241)) ;
#23537 = CARTESIAN_POINT('',(-21.3857615099479,2.3,-1.27440068213391)) ;
#23538 = CARTESIAN_POINT('Origin',(-21.7826790097398,2.3,-1.06835093484243)) ;
#23539 = CARTESIAN_POINT('',(-21.9148668248458,2.55,-1.16439100420103)) ;
#23540 = CARTESIAN_POINT('',(-21.9148668248458,2.3,-1.16439100420103)) ;
#23541 = CARTESIAN_POINT('',(-21.6208756108648,2.55,-0.950793884383935)) ;
#23542 = CARTESIAN_POINT('',(-21.6208756108648,2.3,-0.950793884383935)) ;
#23543 = CARTESIAN_POINT('',(-21.7826790097398,2.55,-1.06835093484243)) ;
#23544 = CARTESIAN_POINT('Origin',(-21.6651219592813,2.55,-1.23015433371742)) ;
#23545 = CARTESIAN_POINT('Origin',(-23.,2.55,-2.2)) ;
#23546 = CARTESIAN_POINT('',(-21.5033185604063,2.55,-1.11259728325892)) ;
#23547 = CARTESIAN_POINT('Origin',(-21.5033185604063,2.3,-1.11259728325892)) ;
#23548 = CARTESIAN_POINT('Origin',(-21.35,2.05,-2.2)) ;
#23549 = CARTESIAN_POINT('',(-21.5133931252681,2.05,-2.4)) ;
#23550 = CARTESIAN_POINT('',(-21.5133931252681,2.05,-2.)) ;
#23551 = CARTESIAN_POINT('Origin',(-23.,2.05,-2.2)) ;
#23552 = CARTESIAN_POINT('',(-21.15,2.05,-2.4)) ;
#23553 = CARTESIAN_POINT('',(-21.35,2.05,-2.4)) ;
#23554 = CARTESIAN_POINT('',(-21.15,2.05,-2.)) ;
#23555 = CARTESIAN_POINT('',(-21.15,2.05,-2.2)) ;
#23556 = CARTESIAN_POINT('',(-21.35,2.05,-2.)) ;
#23557 = CARTESIAN_POINT('Origin',(-21.35,2.3,-2.4)) ;
#23558 = CARTESIAN_POINT('',(-21.5133931252681,2.55,-2.4)) ;
#23559 = CARTESIAN_POINT('',(-21.5133931252681,2.3,-2.4)) ;
#23560 = CARTESIAN_POINT('',(-21.15,2.55,-2.4)) ;
#23561 = CARTESIAN_POINT('',(-21.35,2.55,-2.4)) ;
#23562 = CARTESIAN_POINT('',(-21.15,2.3,-2.4)) ;
#23563 = CARTESIAN_POINT('Origin',(-21.35,2.3,-2.)) ;
#23564 = CARTESIAN_POINT('',(-21.5133931252681,2.55,-2.)) ;
#23565 = CARTESIAN_POINT('',(-21.5133931252681,2.3,-2.)) ;
#23566 = CARTESIAN_POINT('',(-21.15,2.55,-2.)) ;
#23567 = CARTESIAN_POINT('',(-21.15,2.3,-2.)) ;
#23568 = CARTESIAN_POINT('',(-21.35,2.55,-2.)) ;
#23569 = CARTESIAN_POINT('Origin',(-21.35,2.55,-2.2)) ;
#23570 = CARTESIAN_POINT('Origin',(-23.,2.55,-2.2)) ;
#23571 = CARTESIAN_POINT('',(-21.15,2.55,-2.2)) ;
#23572 = CARTESIAN_POINT('Origin',(-21.15,2.3,-2.2)) ;
#23573 = CARTESIAN_POINT('Origin',(-23.,2.3,-2.2)) ;
#23574 = CARTESIAN_POINT('',(-24.5,2.6,-2.2)) ;
#23575 = CARTESIAN_POINT('Origin',(-23.,2.6,-2.2)) ;
#23576 = CARTESIAN_POINT('',(-24.5,2.3,-2.2)) ;
#23577 = CARTESIAN_POINT('',(-24.5,2.,-2.2)) ;
#23578 = CARTESIAN_POINT('',(-24.5,2.3,-2.2)) ;
#23579 = CARTESIAN_POINT('Origin',(-23.,2.,-2.2)) ;
#23580 = CARTESIAN_POINT('Origin',(-23.,2.,-2.2)) ;
#23581 = CARTESIAN_POINT('Origin',(-23.,2.6,-2.2)) ;
#23582 = CARTESIAN_POINT('',(0.,0.,0.)) ;
#23583 = CARTESIAN_POINT('Origin',(-23.,-1.8,-5.75)) ;
#23584 = CARTESIAN_POINT('',(-24.,-1.8,-7.5)) ;
#23585 = CARTESIAN_POINT('Origin',(-23.,-1.8,-7.5)) ;
#23586 = CARTESIAN_POINT('',(-24.,-1.8,-4.)) ;
#23587 = CARTESIAN_POINT('',(-24.,-1.8,-5.75)) ;
#23588 = CARTESIAN_POINT('Origin',(-23.,-1.8,-4.)) ;
#23589 = CARTESIAN_POINT('Origin',(-23.,-1.8,-5.75)) ;
#23590 = CARTESIAN_POINT('',(-24.29,-1.8,-4.)) ;
#23591 = CARTESIAN_POINT('Origin',(-23.,-1.8,-4.)) ;
#23592 = CARTESIAN_POINT('',(-24.29,-1.8,-7.5)) ;
#23593 = CARTESIAN_POINT('',(-24.29,-1.8,-5.75)) ;
#23594 = CARTESIAN_POINT('Origin',(-23.,-1.8,-7.5)) ;
#23595 = CARTESIAN_POINT('Origin',(-23.,-1.8,-7.5)) ;
#23596 = CARTESIAN_POINT('Origin',(-23.,-1.8,-4.)) ;
#23597 = CARTESIAN_POINT('',(0.,0.,0.)) ;
#23598 = CARTESIAN_POINT('Origin',(8.,-7.4,-8.)) ;
#23599 = CARTESIAN_POINT('',(9.4,-7.4,-8.)) ;
#23600 = CARTESIAN_POINT('',(9.23,-7.4,-8.)) ;
#23601 = CARTESIAN_POINT('',(8.,-7.4,-8.)) ;
#23602 = CARTESIAN_POINT('',(6.6,-7.4,-8.)) ;
#23603 = CARTESIAN_POINT('Origin',(8.,-7.4,-8.)) ;
#23604 = CARTESIAN_POINT('',(6.77,-7.4,-8.)) ;
#23605 = CARTESIAN_POINT('',(8.,-7.4,-8.)) ;
#23606 = CARTESIAN_POINT('Origin',(8.,-7.4,-8.)) ;
#23607 = CARTESIAN_POINT('Origin',(8.,-6.,-8.)) ;
#23608 = CARTESIAN_POINT('',(6.6,-4.6,-8.)) ;
#23609 = CARTESIAN_POINT('Origin',(8.,-4.6,-8.)) ;
#23610 = CARTESIAN_POINT('',(6.6,-6.,-8.)) ;
#23611 = CARTESIAN_POINT('Origin',(8.,-7.4,-8.)) ;
#23612 = CARTESIAN_POINT('Origin',(8.,-6.,-8.)) ;
#23613 = CARTESIAN_POINT('',(9.23,-6.73134463286384,-8.)) ;
#23614 = CARTESIAN_POINT('',(9.23,-6.,-8.)) ;
#23615 = CARTESIAN_POINT('',(6.77,-6.73134463286384,-8.)) ;
#23616 = CARTESIAN_POINT('',(6.77,-6.,-8.)) ;
#23617 = CARTESIAN_POINT('',(6.77,-4.6,-8.)) ;
#23618 = CARTESIAN_POINT('',(6.77,-6.,-8.)) ;
#23619 = CARTESIAN_POINT('Origin',(8.,-4.6,-8.)) ;
#23620 = CARTESIAN_POINT('Ctrl Pts',(9.23,-6.73134463286384,-8.)) ;
#23621 = CARTESIAN_POINT('Ctrl Pts',(9.23,-6.73134463286384,-8.08780604230112)) ;
#23622 = CARTESIAN_POINT('Ctrl Pts',(9.22072799863506,-6.71377567825997,-8.17157966039377)) ;
#23623 = CARTESIAN_POINT('Ctrl Pts',(9.18717385924031,-6.65723564339427,-8.33201605328968)) ;
#23624 = CARTESIAN_POINT('Ctrl Pts',(9.16282342807417,-6.61855579361812,-8.40876702722022)) ;
#23625 = CARTESIAN_POINT('Ctrl Pts',(9.10036397056989,-6.53281362355673,-8.55538171579166)) ;
#23626 = CARTESIAN_POINT('Ctrl Pts',(9.06220933130718,-6.48575698731823,-8.62513175063278)) ;
#23627 = CARTESIAN_POINT('Ctrl Pts',(8.97399636293542,-6.39229962882938,-8.75525456150379)) ;
#23628 = CARTESIAN_POINT('Ctrl Pts',(8.92390015166212,-6.3458722876066,-8.81558253005679)) ;
#23629 = CARTESIAN_POINT('Ctrl Pts',(8.76786334513407,-6.22216790150124,-8.97161933658483)) ;
#23630 = CARTESIAN_POINT('Ctrl Pts',(8.63606117977349,-6.14254167736889,-9.06545127512159)) ;
#23631 = CARTESIAN_POINT('Ctrl Pts',(8.41018345337793,-6.05903266002601,-9.16248210994164)) ;
#23632 = CARTESIAN_POINT('Ctrl Pts',(8.33024026117397,-6.03696421286031,-9.18778520433019)) ;
#23633 = CARTESIAN_POINT('Ctrl Pts',(8.16644432291491,-6.00744067465883,-9.22155172186516)) ;
#23634 = CARTESIAN_POINT('Ctrl Pts',(8.08258585694218,-6.,-9.23)) ;
#23635 = CARTESIAN_POINT('Ctrl Pts',(7.91741414305782,-6.,-9.23)) ;
#23636 = CARTESIAN_POINT('Ctrl Pts',(7.83355567708509,-6.00744067465883,-9.22155172186516)) ;
#23637 = CARTESIAN_POINT('Ctrl Pts',(7.66975973882603,-6.0369642128603,-9.18778520433019)) ;
#23638 = CARTESIAN_POINT('Ctrl Pts',(7.58981654662208,-6.05903266002601,-9.16248210994164)) ;
#23639 = CARTESIAN_POINT('Ctrl Pts',(7.36393882022652,-6.14254167736889,-9.06545127512159)) ;
#23640 = CARTESIAN_POINT('Ctrl Pts',(7.23213665486593,-6.22216790150124,-8.97161933658483)) ;
#23641 = CARTESIAN_POINT('Ctrl Pts',(7.07609984833788,-6.3458722876066,-8.81558253005679)) ;
#23642 = CARTESIAN_POINT('Ctrl Pts',(7.02600363706458,-6.39229962882937,-8.75525456150379)) ;
#23643 = CARTESIAN_POINT('Ctrl Pts',(6.93779066869282,-6.48575698731822,-8.62513175063279)) ;
#23644 = CARTESIAN_POINT('Ctrl Pts',(6.89963602943012,-6.53281362355673,-8.55538171579166)) ;
#23645 = CARTESIAN_POINT('Ctrl Pts',(6.83717657192583,-6.61855579361812,-8.40876702722023)) ;
#23646 = CARTESIAN_POINT('Ctrl Pts',(6.81282614075969,-6.65723564339427,-8.33201605328968)) ;
#23647 = CARTESIAN_POINT('Ctrl Pts',(6.77927200136494,-6.71377567825997,-8.17157966039377)) ;
#23648 = CARTESIAN_POINT('Ctrl Pts',(6.77,-6.73134463286384,-8.08780604230112)) ;
#23649 = CARTESIAN_POINT('Ctrl Pts',(6.77,-6.73134463286384,-8.)) ;
#23650 = CARTESIAN_POINT('Origin',(8.,-4.6,-8.)) ;
#23651 = CARTESIAN_POINT('Origin',(8.,-7.4,-9.)) ;
#23652 = CARTESIAN_POINT('Origin',(8.,-7.4,-8.)) ;
#23653 = CARTESIAN_POINT('',(6.6,-7.4,-8.6)) ;
#23654 = CARTESIAN_POINT('',(6.6,-7.4,-9.)) ;
#23655 = CARTESIAN_POINT('',(8.,-8.8,-10.)) ;
#23656 = CARTESIAN_POINT('Origin',(8.,-7.4,-10.)) ;
#23657 = CARTESIAN_POINT('',(8.,-6.,-10.)) ;
#23658 = CARTESIAN_POINT('Origin',(8.,-7.4,-10.)) ;
#23659 = CARTESIAN_POINT('Origin',(8.,-7.4,-10.)) ;
#23660 = CARTESIAN_POINT('Origin',(8.,-7.4,-9.)) ;
#23661 = CARTESIAN_POINT('Origin',(8.,-7.4,-8.)) ;
#23662 = CARTESIAN_POINT('Origin',(-23.,-1.8,-7.8)) ;
#23663 = CARTESIAN_POINT('',(-24.31,-1.8,-7.8)) ;
#23664 = CARTESIAN_POINT('Origin',(-23.,-1.8,-7.8)) ;
#23665 = CARTESIAN_POINT('Origin',(8.,-7.4,-10.)) ;
#23666 = CARTESIAN_POINT('Origin',(8.,-7.4,-10.)) ;
#23667 = CARTESIAN_POINT('Origin',(-23.,-7.4,-10.)) ;
#23668 = CARTESIAN_POINT('',(-23.,-7.20201010126786,-11.3859292911256)) ;
#23669 = CARTESIAN_POINT('',(-23.,-8.02609903369994,-11.2521980673999)) ;
#23670 = CARTESIAN_POINT('Origin',(-23.,-7.4,-10.)) ;
#23671 = CARTESIAN_POINT('',(-23.8082903768655,-8.20829037686548,-10.8082903768655)) ;
#23672 = CARTESIAN_POINT('Origin',(-23.,-7.4,-10.)) ;
#23673 = CARTESIAN_POINT('',(-23.,-7.59798989873238,-8.61407070887439)) ;
#23674 = CARTESIAN_POINT('Origin',(-23.,-7.4,-10.)) ;
#23675 = CARTESIAN_POINT('',(-24.4,-7.40000000000007,-10.)) ;
#23676 = CARTESIAN_POINT('Origin',(-23.,-7.4,-10.)) ;
#23677 = CARTESIAN_POINT('Origin',(-23.,-7.4,-10.)) ;
#23678 = CARTESIAN_POINT('Origin',(-23.,-1.8,-9.2)) ;
#23679 = CARTESIAN_POINT('',(-21.6,-1.8,-9.2)) ;
#23680 = CARTESIAN_POINT('',(-24.4,-1.8,-9.2)) ;
#23681 = CARTESIAN_POINT('Origin',(-23.,-1.8,-9.2)) ;
#23682 = CARTESIAN_POINT('Origin',(-23.,-1.8,-9.2)) ;
#23683 = CARTESIAN_POINT('Origin',(8.,-7.4,-8.)) ;
#23684 = CARTESIAN_POINT('Origin',(-7.5,-7.4,-10.)) ;
#23685 = CARTESIAN_POINT('',(-22.8020101012678,-7.4,-8.6)) ;
#23686 = CARTESIAN_POINT('',(-7.5,-7.4,-8.6)) ;
#23687 = CARTESIAN_POINT('Origin',(-23.,-7.4,-10.)) ;
#23688 = CARTESIAN_POINT('Origin',(-23.,-7.4,-10.)) ;
#23689 = CARTESIAN_POINT('Origin',(-23.,-4.6,-9.6)) ;
#23690 = CARTESIAN_POINT('',(-24.4,-4.6,-9.6)) ;
#23691 = CARTESIAN_POINT('Origin',(-23.,-1.8,-9.2)) ;
#23692 = CARTESIAN_POINT('Origin',(-23.,-1.8,-7.)) ;
#23693 = CARTESIAN_POINT('',(-24.31,-1.8,-6.2)) ;
#23694 = CARTESIAN_POINT('',(-24.31,-1.8,-7.)) ;
#23695 = CARTESIAN_POINT('Origin',(-23.,-1.8,-6.2)) ;
#23696 = CARTESIAN_POINT('Origin',(-23.,-1.8,-7.)) ;
#23697 = CARTESIAN_POINT('',(-24.4,-1.8,-6.2)) ;
#23698 = CARTESIAN_POINT('Origin',(-23.,-1.8,-6.2)) ;
#23699 = CARTESIAN_POINT('',(-24.4,-1.8,-7.)) ;
#23700 = CARTESIAN_POINT('Origin',(-23.,-1.8,-6.2)) ;
#23701 = CARTESIAN_POINT('',(0.,0.,0.)) ;
#23702 = CARTESIAN_POINT('Origin',(-21.2,-2.2,-6.9)) ;
#23703 = CARTESIAN_POINT('',(-21.2963274962599,-2.2,-7.2)) ;
#23704 = CARTESIAN_POINT('',(-21.2963274962599,-2.2,-6.6)) ;
#23705 = CARTESIAN_POINT('',(-21.2963274962599,-2.2,-6.9)) ;
#23706 = CARTESIAN_POINT('',(-20.8,-2.2,-7.2)) ;
#23707 = CARTESIAN_POINT('',(-21.2,-2.2,-7.2)) ;
#23708 = CARTESIAN_POINT('',(-20.8,-2.2,-6.6)) ;
#23709 = CARTESIAN_POINT('',(-20.8,-2.2,-6.9)) ;
#23710 = CARTESIAN_POINT('',(-21.2,-2.2,-6.6)) ;
#23711 = CARTESIAN_POINT('Origin',(-21.6,-1.8,-6.9)) ;
#23712 = CARTESIAN_POINT('',(-21.6,-1.96763054614242,-6.6)) ;
#23713 = CARTESIAN_POINT('',(-21.6,-1.96763054614242,-7.2)) ;
#23714 = CARTESIAN_POINT('',(-21.6,-1.96763054614242,-6.9)) ;
#23715 = CARTESIAN_POINT('',(-21.6,-1.63236945385758,-6.6)) ;
#23716 = CARTESIAN_POINT('',(-21.6,-1.8,-6.6)) ;
#23717 = CARTESIAN_POINT('',(-21.6,-1.63236945385758,-7.2)) ;
#23718 = CARTESIAN_POINT('',(-21.6,-1.63236945385758,-6.9)) ;
#23719 = CARTESIAN_POINT('',(-21.6,-1.8,-7.2)) ;
#23720 = CARTESIAN_POINT('Origin',(-21.2,-1.4,-6.9)) ;
#23721 = CARTESIAN_POINT('',(-21.2963274962599,-1.4,-6.6)) ;
#23722 = CARTESIAN_POINT('',(-21.2963274962599,-1.4,-7.2)) ;
#23723 = CARTESIAN_POINT('',(-21.2963274962599,-1.4,-6.9)) ;
#23724 = CARTESIAN_POINT('',(-20.8,-1.4,-6.6)) ;
#23725 = CARTESIAN_POINT('',(-21.2,-1.4,-6.6)) ;
#23726 = CARTESIAN_POINT('',(-20.8,-1.4,-7.2)) ;
#23727 = CARTESIAN_POINT('',(-20.8,-1.4,-6.9)) ;
#23728 = CARTESIAN_POINT('',(-21.2,-1.4,-7.2)) ;
#23729 = CARTESIAN_POINT('Origin',(-20.8,-1.8,-6.9)) ;
#23730 = CARTESIAN_POINT('',(-20.8,-1.8,-7.2)) ;
#23731 = CARTESIAN_POINT('',(-20.8,-1.8,-6.6)) ;
#23732 = CARTESIAN_POINT('Origin',(-23.,-1.8,-7.2)) ;
#23733 = CARTESIAN_POINT('Origin',(-23.,-1.8,-7.2)) ;
#23734 = CARTESIAN_POINT('Origin',(-23.,-1.8,-7.2)) ;
#23735 = CARTESIAN_POINT('Origin',(-23.,-1.8,-6.9)) ;
#23736 = CARTESIAN_POINT('Origin',(-23.,-1.8,-6.6)) ;
#23737 = CARTESIAN_POINT('Origin',(-23.,-1.8,-6.9)) ;
#23738 = CARTESIAN_POINT('Origin',(-23.,-1.8,-6.6)) ;
#23739 = CARTESIAN_POINT('Origin',(-23.,-1.8,-6.6)) ;
#23740 = CARTESIAN_POINT('',(0.,0.,0.)) ;
#23741 = CARTESIAN_POINT('Origin',(9.8,-5.4,-7.6)) ;
#23742 = CARTESIAN_POINT('',(9.70367250374008,-5.7,-7.6)) ;
#23743 = CARTESIAN_POINT('',(9.70367250374008,-5.1,-7.6)) ;
#23744 = CARTESIAN_POINT('',(9.70367250374008,-5.4,-7.6)) ;
#23745 = CARTESIAN_POINT('',(10.2,-5.7,-7.6)) ;
#23746 = CARTESIAN_POINT('',(9.8,-5.7,-7.6)) ;
#23747 = CARTESIAN_POINT('',(10.2,-5.1,-7.6)) ;
#23748 = CARTESIAN_POINT('',(10.2,-5.4,-7.6)) ;
#23749 = CARTESIAN_POINT('',(9.8,-5.1,-7.6)) ;
#23750 = CARTESIAN_POINT('Origin',(9.4,-5.4,-8.)) ;
#23751 = CARTESIAN_POINT('',(9.4,-5.7,-8.1676305461424)) ;
#23752 = CARTESIAN_POINT('',(9.4,-5.1,-8.1676305461424)) ;
#23753 = CARTESIAN_POINT('',(9.4,-5.4,-8.1676305461424)) ;
#23754 = CARTESIAN_POINT('',(9.4,-5.7,-7.8323694538576)) ;
#23755 = CARTESIAN_POINT('',(9.4,-5.7,-8.)) ;
#23756 = CARTESIAN_POINT('',(9.4,-5.1,-7.8323694538576)) ;
#23757 = CARTESIAN_POINT('',(9.4,-5.4,-7.8323694538576)) ;
#23758 = CARTESIAN_POINT('',(9.4,-5.1,-8.)) ;
#23759 = CARTESIAN_POINT('Origin',(9.8,-5.4,-8.4)) ;
#23760 = CARTESIAN_POINT('',(9.70367250374008,-5.1,-8.4)) ;
#23761 = CARTESIAN_POINT('',(9.70367250374008,-5.7,-8.4)) ;
#23762 = CARTESIAN_POINT('',(9.70367250374008,-5.4,-8.4)) ;
#23763 = CARTESIAN_POINT('',(10.2,-5.1,-8.4)) ;
#23764 = CARTESIAN_POINT('',(9.8,-5.1,-8.4)) ;
#23765 = CARTESIAN_POINT('',(10.2,-5.7,-8.4)) ;
#23766 = CARTESIAN_POINT('',(10.2,-5.4,-8.4)) ;
#23767 = CARTESIAN_POINT('',(9.8,-5.7,-8.4)) ;
#23768 = CARTESIAN_POINT('Origin',(10.2,-5.4,-8.)) ;
#23769 = CARTESIAN_POINT('',(10.2,-5.7,-8.)) ;
#23770 = CARTESIAN_POINT('',(10.2,-5.1,-8.)) ;
#23771 = CARTESIAN_POINT('Origin',(8.,-5.4,-8.)) ;
#23772 = CARTESIAN_POINT('Origin',(8.,-5.7,-8.)) ;
#23773 = CARTESIAN_POINT('Origin',(8.,-5.1,-8.)) ;
#23774 = CARTESIAN_POINT('Origin',(8.,-5.4,-8.)) ;
#23775 = CARTESIAN_POINT('Origin',(8.,-5.1,-8.)) ;
#23776 = CARTESIAN_POINT('Origin',(8.,-5.7,-8.)) ;
#23777 = CARTESIAN_POINT('Origin',(8.,-5.7,-8.)) ;
#23778 = CARTESIAN_POINT('Origin',(8.,-5.1,-8.)) ;
#23779 = CARTESIAN_POINT('',(0.,0.,0.)) ;
#23780 = CARTESIAN_POINT('',(0.,0.,0.)) ;
#23781 = CARTESIAN_POINT('',(0.,0.,0.)) ;
#23782 = CARTESIAN_POINT('',(0.,0.,0.)) ;
#23783 = CARTESIAN_POINT('',(0.,0.,0.)) ;
#23784 = CARTESIAN_POINT('',(0.,0.,0.)) ;
#23785 = CARTESIAN_POINT('',(0.,5.2,0.)) ;
#23786 = CARTESIAN_POINT('',(0.,0.,0.)) ;
#23787 = CARTESIAN_POINT('',(0.,0.,0.)) ;
#23788 = CARTESIAN_POINT('',(0.,0.,0.)) ;
#23789 = CARTESIAN_POINT('',(0.,0.,0.)) ;
#23790 = CARTESIAN_POINT('',(0.,0.,0.)) ;
#23791 = CARTESIAN_POINT('',(0.,0.,0.)) ;
#23792 = CARTESIAN_POINT('',(0.,0.,0.)) ;
#23793 = CARTESIAN_POINT('Origin',(-3.,-1.8,-15.55)) ;
#23794 = CARTESIAN_POINT('',(-3.,-2.9,-15.5552778186154)) ;
#23795 = CARTESIAN_POINT('',(-1.9,-1.8,-15.05)) ;
#23796 = CARTESIAN_POINT('Ctrl Pts',(-3.,-2.9,-15.5552778186154)) ;
#23797 = CARTESIAN_POINT('Ctrl Pts',(-2.92593472403003,-2.9,-15.5552778186154)) ;
#23798 = CARTESIAN_POINT('Ctrl Pts',(-2.85172404139738,-2.89244970013866,
-15.5463012974331)) ;
#23799 = CARTESIAN_POINT('Ctrl Pts',(-2.70730976928893,-2.86290382536062,
-15.5134793386501)) ;
#23800 = CARTESIAN_POINT('Ctrl Pts',(-2.6370687680745,-2.84092482077356,-15.4897837774916)) ;
#23801 = CARTESIAN_POINT('Ctrl Pts',(-2.43708115985337,-2.75608431930036,
-15.4070006970031)) ;
#23802 = CARTESIAN_POINT('Ctrl Pts',(-2.31772068603768,-2.67335560464808,
-15.3370016719564)) ;
#23803 = CARTESIAN_POINT('Ctrl Pts',(-2.12879302508191,-2.48442794369232,
-15.2169163796472)) ;
#23804 = CARTESIAN_POINT('Ctrl Pts',(-2.04479613304032,-2.36484101063073,
-15.1570971235734)) ;
#23805 = CARTESIAN_POINT('Ctrl Pts',(-1.95889743356179,-2.16258851937244,
-15.0942927158064)) ;
#23806 = CARTESIAN_POINT('Ctrl Pts',(-1.93671733228809,-2.09139288005492,
-15.0776864580625)) ;
#23807 = CARTESIAN_POINT('Ctrl Pts',(-1.90726216861058,-1.94630062852708,
-15.0555340958438)) ;
#23808 = CARTESIAN_POINT('Ctrl Pts',(-1.9,-1.87239956586708,-15.05)) ;
#23809 = CARTESIAN_POINT('Ctrl Pts',(-1.9,-1.8,-15.05)) ;
#23810 = CARTESIAN_POINT('',(-4.1,-1.8,-15.05)) ;
#23811 = CARTESIAN_POINT('Ctrl Pts',(-4.1,-1.8,-15.05)) ;
#23812 = CARTESIAN_POINT('Ctrl Pts',(-4.1,-1.87239956586708,-15.05)) ;
#23813 = CARTESIAN_POINT('Ctrl Pts',(-4.09273783138942,-1.94630062852708,
-15.0555340958438)) ;
#23814 = CARTESIAN_POINT('Ctrl Pts',(-4.06328266771191,-2.09139288005492,
-15.0776864580625)) ;
#23815 = CARTESIAN_POINT('Ctrl Pts',(-4.04110256643821,-2.16258851937244,
-15.0942927158064)) ;
#23816 = CARTESIAN_POINT('Ctrl Pts',(-3.95520386695968,-2.36484101063073,
-15.1570971235734)) ;
#23817 = CARTESIAN_POINT('Ctrl Pts',(-3.87120697491809,-2.48442794369232,
-15.2169163796472)) ;
#23818 = CARTESIAN_POINT('Ctrl Pts',(-3.68227931396233,-2.67335560464808,
-15.3370016719564)) ;
#23819 = CARTESIAN_POINT('Ctrl Pts',(-3.56291884014663,-2.75608431930036,
-15.4070006970031)) ;
#23820 = CARTESIAN_POINT('Ctrl Pts',(-3.3629312319255,-2.84092482077356,-15.4897837774916)) ;
#23821 = CARTESIAN_POINT('Ctrl Pts',(-3.29269023071107,-2.86290382536062,
-15.5134793386501)) ;
#23822 = CARTESIAN_POINT('Ctrl Pts',(-3.14827595860262,-2.89244970013866,
-15.5463012974331)) ;
#23823 = CARTESIAN_POINT('Ctrl Pts',(-3.07406527596997,-2.9,-15.5552778186154)) ;
#23824 = CARTESIAN_POINT('Ctrl Pts',(-3.,-2.9,-15.5552778186154)) ;
#23825 = CARTESIAN_POINT('',(-4.1,-1.8,-14.75)) ;
#23826 = CARTESIAN_POINT('',(-4.1,-1.8,-15.55)) ;
#23827 = CARTESIAN_POINT('',(-3.,-2.9,-15.1389342411184)) ;
#23828 = CARTESIAN_POINT('Ctrl Pts',(-3.,-2.9,-15.1389342411184)) ;
#23829 = CARTESIAN_POINT('Ctrl Pts',(-3.07181116971736,-2.9,-15.1389342411184)) ;
#23830 = CARTESIAN_POINT('Ctrl Pts',(-3.14499752680644,-2.89286661726534,
-15.1330764609861)) ;
#23831 = CARTESIAN_POINT('Ctrl Pts',(-3.28883700701042,-2.86393369738317,
-15.1104380225034)) ;
#23832 = CARTESIAN_POINT('Ctrl Pts',(-3.3595029893093,-2.84215035317734,-15.0937184190741)) ;
#23833 = CARTESIAN_POINT('Ctrl Pts',(-3.56118090687537,-2.75726493295417,
-15.0333835136228)) ;
#23834 = CARTESIAN_POINT('Ctrl Pts',(-3.68198795957211,-2.6736469590383,-14.9799062284422)) ;
#23835 = CARTESIAN_POINT('Ctrl Pts',(-3.87286762925623,-2.48276728935417,
-14.8851973706734)) ;
#23836 = CARTESIAN_POINT('Ctrl Pts',(-3.95701740777658,-2.36176319521959,
-14.8367787014793)) ;
#23837 = CARTESIAN_POINT('Ctrl Pts',(-4.0422651124962,-2.15923323536895,-14.7858537872249)) ;
#23838 = CARTESIAN_POINT('Ctrl Pts',(-4.06409704750744,-2.08825332179439,
-14.7723789472322)) ;
#23839 = CARTESIAN_POINT('Ctrl Pts',(-4.09297019244892,-1.9442520796829,-14.7544468449727)) ;
#23840 = CARTESIAN_POINT('Ctrl Pts',(-4.1,-1.87122716809572,-14.75)) ;
#23841 = CARTESIAN_POINT('Ctrl Pts',(-4.1,-1.8,-14.75)) ;
#23842 = CARTESIAN_POINT('',(-1.9,-1.8,-14.75)) ;
#23843 = CARTESIAN_POINT('Ctrl Pts',(-1.9,-1.8,-14.75)) ;
#23844 = CARTESIAN_POINT('Ctrl Pts',(-1.9,-1.87122716809572,-14.75)) ;
#23845 = CARTESIAN_POINT('Ctrl Pts',(-1.90702980755108,-1.9442520796829,-14.7544468449727)) ;
#23846 = CARTESIAN_POINT('Ctrl Pts',(-1.93590295249256,-2.08825332179439,
-14.7723789472322)) ;
#23847 = CARTESIAN_POINT('Ctrl Pts',(-1.9577348875038,-2.15923323536894,-14.7858537872249)) ;
#23848 = CARTESIAN_POINT('Ctrl Pts',(-2.04298259222342,-2.36176319521959,
-14.8367787014793)) ;
#23849 = CARTESIAN_POINT('Ctrl Pts',(-2.12713237074377,-2.48276728935417,
-14.8851973706734)) ;
#23850 = CARTESIAN_POINT('Ctrl Pts',(-2.31801204042789,-2.6736469590383,-14.9799062284422)) ;
#23851 = CARTESIAN_POINT('Ctrl Pts',(-2.43881909312463,-2.75726493295417,
-15.0333835136228)) ;
#23852 = CARTESIAN_POINT('Ctrl Pts',(-2.6404970106907,-2.84215035317734,-15.0937184190741)) ;
#23853 = CARTESIAN_POINT('Ctrl Pts',(-2.71116299298958,-2.86393369738317,
-15.1104380225034)) ;
#23854 = CARTESIAN_POINT('Ctrl Pts',(-2.85500247319356,-2.89286661726534,
-15.1330764609861)) ;
#23855 = CARTESIAN_POINT('Ctrl Pts',(-2.92818883028264,-2.9,-15.1389342411184)) ;
#23856 = CARTESIAN_POINT('Ctrl Pts',(-3.,-2.9,-15.1389342411184)) ;
#23857 = CARTESIAN_POINT('Ctrl Pts',(-4.1,-1.8,-14.75)) ;
#23858 = CARTESIAN_POINT('Ctrl Pts',(-4.1,-1.72877283190428,-14.75)) ;
#23859 = CARTESIAN_POINT('Ctrl Pts',(-4.09297019244892,-1.6557479203171,-14.7544468449727)) ;
#23860 = CARTESIAN_POINT('Ctrl Pts',(-4.06409704750744,-1.51174667820561,
-14.7723789472322)) ;
#23861 = CARTESIAN_POINT('Ctrl Pts',(-4.0422651124962,-1.44076676463106,-14.7858537872249)) ;
#23862 = CARTESIAN_POINT('Ctrl Pts',(-3.95701740777658,-1.23823680478041,
-14.8367787014793)) ;
#23863 = CARTESIAN_POINT('Ctrl Pts',(-3.87286762925623,-1.11723271064583,
-14.8851973706734)) ;
#23864 = CARTESIAN_POINT('Ctrl Pts',(-3.68198795957211,-0.926353040961702,
-14.9799062284422)) ;
#23865 = CARTESIAN_POINT('Ctrl Pts',(-3.56118090687537,-0.842735067045828,
-15.0333835136228)) ;
#23866 = CARTESIAN_POINT('Ctrl Pts',(-3.3595029893093,-0.757849646822659,
-15.0937184190741)) ;
#23867 = CARTESIAN_POINT('Ctrl Pts',(-3.28883700701042,-0.736066302616833,
-15.1104380225034)) ;
#23868 = CARTESIAN_POINT('Ctrl Pts',(-3.14499752680644,-0.707133382734658,
-15.1330764609861)) ;
#23869 = CARTESIAN_POINT('Ctrl Pts',(-3.07181116971736,-0.7,-15.1389342411184)) ;
#23870 = CARTESIAN_POINT('Ctrl Pts',(-2.92818883028264,-0.7,-15.1389342411184)) ;
#23871 = CARTESIAN_POINT('Ctrl Pts',(-2.85500247319356,-0.707133382734658,
-15.1330764609861)) ;
#23872 = CARTESIAN_POINT('Ctrl Pts',(-2.71116299298958,-0.736066302616833,
-15.1104380225034)) ;
#23873 = CARTESIAN_POINT('Ctrl Pts',(-2.6404970106907,-0.75784964682266,-15.0937184190741)) ;
#23874 = CARTESIAN_POINT('Ctrl Pts',(-2.43881909312463,-0.842735067045828,
-15.0333835136228)) ;
#23875 = CARTESIAN_POINT('Ctrl Pts',(-2.31801204042789,-0.926353040961702,
-14.9799062284422)) ;
#23876 = CARTESIAN_POINT('Ctrl Pts',(-2.12713237074376,-1.11723271064583,
-14.8851973706734)) ;
#23877 = CARTESIAN_POINT('Ctrl Pts',(-2.04298259222342,-1.23823680478041,
-14.8367787014793)) ;
#23878 = CARTESIAN_POINT('Ctrl Pts',(-1.9577348875038,-1.44076676463106,-14.7858537872249)) ;
#23879 = CARTESIAN_POINT('Ctrl Pts',(-1.93590295249256,-1.51174667820561,
-14.7723789472322)) ;
#23880 = CARTESIAN_POINT('Ctrl Pts',(-1.90702980755108,-1.6557479203171,-14.7544468449727)) ;
#23881 = CARTESIAN_POINT('Ctrl Pts',(-1.9,-1.72877283190428,-14.75)) ;
#23882 = CARTESIAN_POINT('Ctrl Pts',(-1.9,-1.8,-14.75)) ;
#23883 = CARTESIAN_POINT('Ctrl Pts',(-1.9,-1.8,-15.05)) ;
#23884 = CARTESIAN_POINT('Ctrl Pts',(-1.9,-1.72760043413292,-15.05)) ;
#23885 = CARTESIAN_POINT('Ctrl Pts',(-1.90726216861058,-1.65369937147292,
-15.0555340958438)) ;
#23886 = CARTESIAN_POINT('Ctrl Pts',(-1.93671733228809,-1.50860711994508,
-15.0776864580625)) ;
#23887 = CARTESIAN_POINT('Ctrl Pts',(-1.95889743356178,-1.43741148062756,
-15.0942927158064)) ;
#23888 = CARTESIAN_POINT('Ctrl Pts',(-2.04479613304032,-1.23515898936927,
-15.1570971235734)) ;
#23889 = CARTESIAN_POINT('Ctrl Pts',(-2.12879302508191,-1.11557205630768,
-15.2169163796472)) ;
#23890 = CARTESIAN_POINT('Ctrl Pts',(-2.31772068603768,-0.92664439535192,
-15.3370016719564)) ;
#23891 = CARTESIAN_POINT('Ctrl Pts',(-2.43708115985337,-0.843915680699641,
-15.4070006970031)) ;
#23892 = CARTESIAN_POINT('Ctrl Pts',(-2.6370687680745,-0.759075179226438,
-15.4897837774916)) ;
#23893 = CARTESIAN_POINT('Ctrl Pts',(-2.70730976928893,-0.737096174639381,
-15.5134793386501)) ;
#23894 = CARTESIAN_POINT('Ctrl Pts',(-2.85172404139738,-0.707550299861341,
-15.5463012974331)) ;
#23895 = CARTESIAN_POINT('Ctrl Pts',(-2.92593472403003,-0.7,-15.5552778186154)) ;
#23896 = CARTESIAN_POINT('Ctrl Pts',(-3.07406527596997,-0.7,-15.5552778186154)) ;
#23897 = CARTESIAN_POINT('Ctrl Pts',(-3.14827595860262,-0.707550299861341,
-15.5463012974331)) ;
#23898 = CARTESIAN_POINT('Ctrl Pts',(-3.29269023071107,-0.737096174639381,
-15.5134793386501)) ;
#23899 = CARTESIAN_POINT('Ctrl Pts',(-3.3629312319255,-0.759075179226438,
-15.4897837774916)) ;
#23900 = CARTESIAN_POINT('Ctrl Pts',(-3.56291884014663,-0.843915680699641,
-15.4070006970031)) ;
#23901 = CARTESIAN_POINT('Ctrl Pts',(-3.68227931396233,-0.92664439535192,
-15.3370016719564)) ;
#23902 = CARTESIAN_POINT('Ctrl Pts',(-3.87120697491809,-1.11557205630768,
-15.2169163796472)) ;
#23903 = CARTESIAN_POINT('Ctrl Pts',(-3.95520386695968,-1.23515898936927,
-15.1570971235734)) ;
#23904 = CARTESIAN_POINT('Ctrl Pts',(-4.04110256643821,-1.43741148062756,
-15.0942927158064)) ;
#23905 = CARTESIAN_POINT('Ctrl Pts',(-4.06328266771191,-1.50860711994508,
-15.0776864580625)) ;
#23906 = CARTESIAN_POINT('Ctrl Pts',(-4.09273783138942,-1.65369937147292,
-15.0555340958438)) ;
#23907 = CARTESIAN_POINT('Ctrl Pts',(-4.1,-1.72760043413292,-15.05)) ;
#23908 = CARTESIAN_POINT('Ctrl Pts',(-4.1,-1.8,-15.05)) ;
#23909 = CARTESIAN_POINT('Origin',(-11.,-1.8,-16.5)) ;
#23910 = CARTESIAN_POINT('',(-30.,-1.8,-15.05)) ;
#23911 = CARTESIAN_POINT('Origin',(-30.,-1.8,-16.5)) ;
#23912 = CARTESIAN_POINT('',(-11.,-1.8,-15.05)) ;
#23913 = CARTESIAN_POINT('',(8.,-1.8,-15.05)) ;
#23914 = CARTESIAN_POINT('',(-11.,-1.8,-15.05)) ;
#23915 = CARTESIAN_POINT('Origin',(8.,-1.8,-16.5)) ;
#23916 = CARTESIAN_POINT('Origin',(-11.,-1.8,-16.5)) ;
#23917 = CARTESIAN_POINT('',(8.,-1.8,-14.75)) ;
#23918 = CARTESIAN_POINT('Origin',(8.,-1.8,-16.5)) ;
#23919 = CARTESIAN_POINT('',(-11.,-1.8,-14.75)) ;
#23920 = CARTESIAN_POINT('',(-30.,-1.8,-14.75)) ;
#23921 = CARTESIAN_POINT('',(-11.,-1.8,-14.75)) ;
#23922 = CARTESIAN_POINT('Origin',(-30.,-1.8,-16.5)) ;
#23923 = CARTESIAN_POINT('Origin',(-30.,-1.8,-16.5)) ;
#23924 = CARTESIAN_POINT('Origin',(8.,-1.8,-16.5)) ;
#23925 = CARTESIAN_POINT('',(0.,0.,0.)) ;
#23926 = CARTESIAN_POINT('Origin',(-3.,-1.8,-16.6)) ;
#23927 = CARTESIAN_POINT('',(-2.14559962546825,-1.10717967697245,-16.6)) ;
#23928 = CARTESIAN_POINT('',(-3.85440037453175,-1.10717967697245,-16.6)) ;
#23929 = CARTESIAN_POINT('',(-4.,-1.10717967697245,-16.6)) ;
#23930 = CARTESIAN_POINT('',(-2.53095842401766,-0.80501256289338,-16.6)) ;
#23931 = CARTESIAN_POINT('Origin',(-3.,-1.8,-16.6)) ;
#23932 = CARTESIAN_POINT('',(-3.46904157598234,-0.80501256289338,-16.6)) ;
#23933 = CARTESIAN_POINT('',(-4.,-0.80501256289338,-16.6)) ;
#23934 = CARTESIAN_POINT('Origin',(-3.,-1.8,-16.6)) ;
#23935 = CARTESIAN_POINT('Origin',(-3.,-1.8,-15.55)) ;
#23936 = CARTESIAN_POINT('',(-4.1,-1.8,-15.8)) ;
#23937 = CARTESIAN_POINT('Ctrl Pts',(-3.85440037453175,-1.10717967697245,
-16.6)) ;
#23938 = CARTESIAN_POINT('Ctrl Pts',(-3.85049705318298,-1.10236602022558,
-16.5666500077769)) ;
#23939 = CARTESIAN_POINT('Ctrl Pts',(-3.84852813742386,-1.1,-16.5331059816471)) ;
#23940 = CARTESIAN_POINT('Ctrl Pts',(-3.84852813742386,-1.1,-16.5)) ;
#23941 = CARTESIAN_POINT('Ctrl Pts',(-3.84852813742386,-1.1,-16.408477950171)) ;
#23942 = CARTESIAN_POINT('Ctrl Pts',(-3.86487430708359,-1.11884674360792,
-16.3138744868034)) ;
#23943 = CARTESIAN_POINT('Ctrl Pts',(-3.91703156085527,-1.19087751926739,
-16.1428129676115)) ;
#23944 = CARTESIAN_POINT('Ctrl Pts',(-3.95162711030062,-1.24406317485413,
-16.0659873314847)) ;
#23945 = CARTESIAN_POINT('Ctrl Pts',(-4.01279528835241,-1.36545967307144,
-15.9445908332674)) ;
#23946 = CARTESIAN_POINT('Ctrl Pts',(-4.04402775497001,-1.44241519978942,
-15.8910472783858)) ;
#23947 = CARTESIAN_POINT('Ctrl Pts',(-4.08782165352582,-1.6142450358863,-15.8186884461636)) ;
#23948 = CARTESIAN_POINT('Ctrl Pts',(-4.1,-1.70927012099139,-15.8)) ;
#23949 = CARTESIAN_POINT('Ctrl Pts',(-4.1,-1.8,-15.8)) ;
#23950 = CARTESIAN_POINT('',(-4.1,-1.8,-15.5)) ;
#23951 = CARTESIAN_POINT('Ctrl Pts',(-4.1,-1.8,-15.5)) ;
#23952 = CARTESIAN_POINT('Ctrl Pts',(-4.1,-1.73245114455087,-15.5)) ;
#23953 = CARTESIAN_POINT('Ctrl Pts',(-4.09366900622909,-1.66396811523288,
-15.5069510256229)) ;
#23954 = CARTESIAN_POINT('Ctrl Pts',(-4.06861417966391,-1.53040715178794,
-15.5346137377671)) ;
#23955 = CARTESIAN_POINT('Ctrl Pts',(-4.04990213252851,-1.46532446507313,
-15.5553131496202)) ;
#23956 = CARTESIAN_POINT('Ctrl Pts',(-3.97908681363415,-1.28173592783325,
-15.6344562293198)) ;
#23957 = CARTESIAN_POINT('Ctrl Pts',(-3.91155673921738,-1.17504680959349,
-15.7107396280334)) ;
#23958 = CARTESIAN_POINT('Ctrl Pts',(-3.76780945986836,-1.00375215686099,
-15.8820342807659)) ;
#23959 = CARTESIAN_POINT('Ctrl Pts',(-3.67938152899323,-0.930008802100376,
-15.9904145776246)) ;
#23960 = CARTESIAN_POINT('Ctrl Pts',(-3.56405332421194,-0.85450777858214,
-16.1680616160286)) ;
#23961 = CARTESIAN_POINT('Ctrl Pts',(-3.52879854306256,-0.834982894950926,
-16.2296167208294)) ;
#23962 = CARTESIAN_POINT('Ctrl Pts',(-3.47583842827067,-0.807798528642412,
-16.3589280031455)) ;
#23963 = CARTESIAN_POINT('Ctrl Pts',(-3.45825756949558,-0.8,-16.4267058609218)) ;
#23964 = CARTESIAN_POINT('Ctrl Pts',(-3.45825756949558,-0.8,-16.5)) ;
#23965 = CARTESIAN_POINT('Ctrl Pts',(-3.45825756949558,-0.8,-16.5344735344061)) ;
#23966 = CARTESIAN_POINT('Ctrl Pts',(-3.46215940235726,-0.801768275133648,
-16.5677197443671)) ;
#23967 = CARTESIAN_POINT('Ctrl Pts',(-3.46904157598234,-0.80501256289338,
-16.6)) ;
#23968 = CARTESIAN_POINT('',(-3.46904157598234,-2.79498743710662,-16.6)) ;
#23969 = CARTESIAN_POINT('Ctrl Pts',(-3.46904157598234,-2.79498743710662,
-16.6)) ;
#23970 = CARTESIAN_POINT('Ctrl Pts',(-3.46215940232543,-2.79823172488136,
-16.5677197442178)) ;
#23971 = CARTESIAN_POINT('Ctrl Pts',(-3.45825756949559,-2.8,-16.5344735330852)) ;
#23972 = CARTESIAN_POINT('Ctrl Pts',(-3.45825756949558,-2.8,-16.4267058609218)) ;
#23973 = CARTESIAN_POINT('Ctrl Pts',(-3.47583842827066,-2.79220147135759,
-16.3589280031455)) ;
#23974 = CARTESIAN_POINT('Ctrl Pts',(-3.52879854306256,-2.76501710504908,
-16.2296167208294)) ;
#23975 = CARTESIAN_POINT('Ctrl Pts',(-3.56405332421193,-2.74549222141786,
-16.1680616160286)) ;
#23976 = CARTESIAN_POINT('Ctrl Pts',(-3.67938152899323,-2.66999119789963,
-15.9904145776246)) ;
#23977 = CARTESIAN_POINT('Ctrl Pts',(-3.76780945986836,-2.59624784313901,
-15.8820342807659)) ;
#23978 = CARTESIAN_POINT('Ctrl Pts',(-3.91155673921738,-2.42495319040651,
-15.7107396280334)) ;
#23979 = CARTESIAN_POINT('Ctrl Pts',(-3.97908681363414,-2.31826407216675,
-15.6344562293198)) ;
#23980 = CARTESIAN_POINT('Ctrl Pts',(-4.04990213252851,-2.13467553492687,
-15.5553131496202)) ;
#23981 = CARTESIAN_POINT('Ctrl Pts',(-4.06861417966391,-2.06959284821206,
-15.5346137377671)) ;
#23982 = CARTESIAN_POINT('Ctrl Pts',(-4.09366900622909,-1.93603188476712,
-15.5069510256229)) ;
#23983 = CARTESIAN_POINT('Ctrl Pts',(-4.1,-1.86754885544913,-15.5)) ;
#23984 = CARTESIAN_POINT('Ctrl Pts',(-4.1,-1.8,-15.5)) ;
#23985 = CARTESIAN_POINT('',(-3.85440037453175,-2.49282032302755,-16.6)) ;
#23986 = CARTESIAN_POINT('Origin',(-3.,-1.8,-16.6)) ;
#23987 = CARTESIAN_POINT('Ctrl Pts',(-4.1,-1.8,-15.8)) ;
#23988 = CARTESIAN_POINT('Ctrl Pts',(-4.1,-1.89072987900861,-15.8)) ;
#23989 = CARTESIAN_POINT('Ctrl Pts',(-4.08782165352582,-1.9857549641137,-15.8186884461636)) ;
#23990 = CARTESIAN_POINT('Ctrl Pts',(-4.04402775497001,-2.15758480021059,
-15.8910472783858)) ;
#23991 = CARTESIAN_POINT('Ctrl Pts',(-4.01279528835241,-2.23454032692856,
-15.9445908332674)) ;
#23992 = CARTESIAN_POINT('Ctrl Pts',(-3.95162711030062,-2.35593682514587,
-16.0659873314847)) ;
#23993 = CARTESIAN_POINT('Ctrl Pts',(-3.91703156085527,-2.40912248073261,
-16.1428129676115)) ;
#23994 = CARTESIAN_POINT('Ctrl Pts',(-3.86487430708359,-2.48115325639208,
-16.3138744868034)) ;
#23995 = CARTESIAN_POINT('Ctrl Pts',(-3.84852813742386,-2.5,-16.408477950171)) ;
#23996 = CARTESIAN_POINT('Ctrl Pts',(-3.84852813742386,-2.5,-16.5331059854704)) ;
#23997 = CARTESIAN_POINT('Ctrl Pts',(-3.85049705337729,-2.4976339795348,-16.5666500094371)) ;
#23998 = CARTESIAN_POINT('Ctrl Pts',(-3.85440037453175,-2.49282032302755,
-16.6)) ;
#23999 = CARTESIAN_POINT('Origin',(-3.,-1.8,-15.55)) ;
#24000 = CARTESIAN_POINT('',(-2.14559962546825,-2.49282032302755,-16.6)) ;
#24001 = CARTESIAN_POINT('',(-1.9,-1.8,-15.8)) ;
#24002 = CARTESIAN_POINT('Ctrl Pts',(-2.14559962546825,-2.49282032302755,
-16.6)) ;
#24003 = CARTESIAN_POINT('Ctrl Pts',(-2.14950294681702,-2.49763397977442,
-16.5666500077769)) ;
#24004 = CARTESIAN_POINT('Ctrl Pts',(-2.15147186257614,-2.5,-16.5331059816471)) ;
#24005 = CARTESIAN_POINT('Ctrl Pts',(-2.15147186257614,-2.5,-16.408477950171)) ;
#24006 = CARTESIAN_POINT('Ctrl Pts',(-2.13512569291641,-2.48115325639208,
-16.3138744868034)) ;
#24007 = CARTESIAN_POINT('Ctrl Pts',(-2.08296843914473,-2.40912248073261,
-16.1428129676115)) ;
#24008 = CARTESIAN_POINT('Ctrl Pts',(-2.04837288969938,-2.35593682514587,
-16.0659873314847)) ;
#24009 = CARTESIAN_POINT('Ctrl Pts',(-1.98720471164759,-2.23454032692856,
-15.9445908332674)) ;
#24010 = CARTESIAN_POINT('Ctrl Pts',(-1.95597224502999,-2.15758480021059,
-15.8910472783858)) ;
#24011 = CARTESIAN_POINT('Ctrl Pts',(-1.91217834647418,-1.9857549641137,-15.8186884461636)) ;
#24012 = CARTESIAN_POINT('Ctrl Pts',(-1.9,-1.89072987900861,-15.8)) ;
#24013 = CARTESIAN_POINT('Ctrl Pts',(-1.9,-1.8,-15.8)) ;
#24014 = CARTESIAN_POINT('',(-2.53095842401766,-2.79498743710662,-16.6)) ;
#24015 = CARTESIAN_POINT('Origin',(-3.,-1.8,-16.6)) ;
#24016 = CARTESIAN_POINT('',(-1.9,-1.8,-15.5)) ;
#24017 = CARTESIAN_POINT('Ctrl Pts',(-1.9,-1.8,-15.5)) ;
#24018 = CARTESIAN_POINT('Ctrl Pts',(-1.9,-1.86754885544913,-15.5)) ;
#24019 = CARTESIAN_POINT('Ctrl Pts',(-1.90633099377091,-1.93603188476712,
-15.5069510256229)) ;
#24020 = CARTESIAN_POINT('Ctrl Pts',(-1.93138582033609,-2.06959284821206,
-15.5346137377671)) ;
#24021 = CARTESIAN_POINT('Ctrl Pts',(-1.95009786747149,-2.13467553492686,
-15.5553131496202)) ;
#24022 = CARTESIAN_POINT('Ctrl Pts',(-2.02091318636585,-2.31826407216675,
-15.6344562293198)) ;
#24023 = CARTESIAN_POINT('Ctrl Pts',(-2.08844326078262,-2.42495319040651,
-15.7107396280334)) ;
#24024 = CARTESIAN_POINT('Ctrl Pts',(-2.23219054013164,-2.59624784313901,
-15.8820342807659)) ;
#24025 = CARTESIAN_POINT('Ctrl Pts',(-2.32061847100677,-2.66999119789963,
-15.9904145776246)) ;
#24026 = CARTESIAN_POINT('Ctrl Pts',(-2.43594667578807,-2.74549222141786,
-16.1680616160286)) ;
#24027 = CARTESIAN_POINT('Ctrl Pts',(-2.47120145693744,-2.76501710504908,
-16.2296167208294)) ;
#24028 = CARTESIAN_POINT('Ctrl Pts',(-2.52416157172934,-2.79220147135759,
-16.3589280031455)) ;
#24029 = CARTESIAN_POINT('Ctrl Pts',(-2.54174243050442,-2.8,-16.4267058609218)) ;
#24030 = CARTESIAN_POINT('Ctrl Pts',(-2.54174243050442,-2.8,-16.5344735344061)) ;
#24031 = CARTESIAN_POINT('Ctrl Pts',(-2.53784059764274,-2.79823172486635,
-16.5677197443671)) ;
#24032 = CARTESIAN_POINT('Ctrl Pts',(-2.53095842401766,-2.79498743710662,
-16.6)) ;
#24033 = CARTESIAN_POINT('Ctrl Pts',(-2.53095842401766,-0.80501256289338,
-16.6)) ;
#24034 = CARTESIAN_POINT('Ctrl Pts',(-2.53784059767457,-0.801768275118644,
-16.5677197442178)) ;
#24035 = CARTESIAN_POINT('Ctrl Pts',(-2.54174243050442,-0.8,-16.5344735330852)) ;
#24036 = CARTESIAN_POINT('Ctrl Pts',(-2.54174243050442,-0.8,-16.5)) ;
#24037 = CARTESIAN_POINT('Ctrl Pts',(-2.54174243050442,-0.8,-16.4267058609218)) ;
#24038 = CARTESIAN_POINT('Ctrl Pts',(-2.52416157172934,-0.807798528642411,
-16.3589280031455)) ;
#24039 = CARTESIAN_POINT('Ctrl Pts',(-2.47120145693744,-0.834982894950924,
-16.2296167208294)) ;
#24040 = CARTESIAN_POINT('Ctrl Pts',(-2.43594667578807,-0.854507778582139,
-16.1680616160286)) ;
#24041 = CARTESIAN_POINT('Ctrl Pts',(-2.32061847100677,-0.930008802100373,
-15.9904145776246)) ;
#24042 = CARTESIAN_POINT('Ctrl Pts',(-2.23219054013164,-1.00375215686099,
-15.8820342807659)) ;
#24043 = CARTESIAN_POINT('Ctrl Pts',(-2.08844326078262,-1.17504680959349,
-15.7107396280334)) ;
#24044 = CARTESIAN_POINT('Ctrl Pts',(-2.02091318636585,-1.28173592783325,
-15.6344562293198)) ;
#24045 = CARTESIAN_POINT('Ctrl Pts',(-1.95009786747149,-1.46532446507313,
-15.5553131496202)) ;
#24046 = CARTESIAN_POINT('Ctrl Pts',(-1.93138582033609,-1.53040715178794,
-15.5346137377671)) ;
#24047 = CARTESIAN_POINT('Ctrl Pts',(-1.90633099377091,-1.66396811523288,
-15.5069510256229)) ;
#24048 = CARTESIAN_POINT('Ctrl Pts',(-1.9,-1.73245114455087,-15.5)) ;
#24049 = CARTESIAN_POINT('Ctrl Pts',(-1.9,-1.8,-15.5)) ;
#24050 = CARTESIAN_POINT('Ctrl Pts',(-1.9,-1.8,-15.8)) ;
#24051 = CARTESIAN_POINT('Ctrl Pts',(-1.9,-1.70927012099139,-15.8)) ;
#24052 = CARTESIAN_POINT('Ctrl Pts',(-1.91217834647418,-1.6142450358863,-15.8186884461636)) ;
#24053 = CARTESIAN_POINT('Ctrl Pts',(-1.95597224502999,-1.44241519978941,
-15.8910472783858)) ;
#24054 = CARTESIAN_POINT('Ctrl Pts',(-1.98720471164759,-1.36545967307144,
-15.9445908332674)) ;
#24055 = CARTESIAN_POINT('Ctrl Pts',(-2.04837288969938,-1.24406317485413,
-16.0659873314847)) ;
#24056 = CARTESIAN_POINT('Ctrl Pts',(-2.08296843914473,-1.19087751926739,
-16.1428129676115)) ;
#24057 = CARTESIAN_POINT('Ctrl Pts',(-2.13512569291641,-1.11884674360792,
-16.3138744868034)) ;
#24058 = CARTESIAN_POINT('Ctrl Pts',(-2.15147186257614,-1.1,-16.408477950171)) ;
#24059 = CARTESIAN_POINT('Ctrl Pts',(-2.15147186257614,-1.1,-16.5)) ;
#24060 = CARTESIAN_POINT('Ctrl Pts',(-2.15147186257614,-1.1,-16.5331059854704)) ;
#24061 = CARTESIAN_POINT('Ctrl Pts',(-2.14950294662271,-1.1023660204652,-16.5666500094371)) ;
#24062 = CARTESIAN_POINT('Ctrl Pts',(-2.14559962546825,-1.10717967697245,
-16.6)) ;
#24063 = CARTESIAN_POINT('Origin',(-3.,-1.8,-16.6)) ;
#24064 = CARTESIAN_POINT('',(-4.,-2.49282032302755,-16.6)) ;
#24065 = CARTESIAN_POINT('',(-4.,-2.79498743710662,-16.6)) ;
#24066 = CARTESIAN_POINT('Origin',(-4.,-1.8,-16.5)) ;
#24067 = CARTESIAN_POINT('',(-9.,-1.8,-15.8)) ;
#24068 = CARTESIAN_POINT('Origin',(-9.,-1.8,-16.5)) ;
#24069 = CARTESIAN_POINT('',(-4.,-1.8,-15.8)) ;
#24070 = CARTESIAN_POINT('',(1.,-1.8,-15.8)) ;
#24071 = CARTESIAN_POINT('',(-4.,-1.8,-15.8)) ;
#24072 = CARTESIAN_POINT('Origin',(1.,-1.8,-16.5)) ;
#24073 = CARTESIAN_POINT('Origin',(0.,-1.8,-16.5)) ;
#24074 = CARTESIAN_POINT('',(1.,-1.8,-15.05)) ;
#24075 = CARTESIAN_POINT('Origin',(1.,-1.8,-16.5)) ;
#24076 = CARTESIAN_POINT('',(-1.,-1.8,-15.5)) ;
#24077 = CARTESIAN_POINT('',(0.,-1.8,-15.275)) ;
#24078 = CARTESIAN_POINT('Origin',(-1.,-1.8,-16.5)) ;
#24079 = CARTESIAN_POINT('Origin',(1.,-1.8,-16.5)) ;
#24080 = CARTESIAN_POINT('Origin',(-4.,-1.8,-16.5)) ;
#24081 = CARTESIAN_POINT('',(-4.,-1.8,-15.5)) ;
#24082 = CARTESIAN_POINT('',(-7.,-1.8,-15.5)) ;
#24083 = CARTESIAN_POINT('',(-4.,-1.8,-15.5)) ;
#24084 = CARTESIAN_POINT('Origin',(-7.,-1.8,-16.5)) ;
#24085 = CARTESIAN_POINT('Origin',(-8.,-1.8,-16.5)) ;
#24086 = CARTESIAN_POINT('',(-9.,-1.8,-15.05)) ;
#24087 = CARTESIAN_POINT('',(-8.,-1.8,-15.275)) ;
#24088 = CARTESIAN_POINT('Origin',(-9.,-1.8,-16.5)) ;
#24089 = CARTESIAN_POINT('Origin',(-9.,-1.8,-16.5)) ;
#24090 = CARTESIAN_POINT('',(0.,0.,0.)) ;
#24091 = CARTESIAN_POINT('Origin',(-3.,-1.8,-13.2)) ;
#24092 = CARTESIAN_POINT('',(-3.85,-1.8,-15.1)) ;
#24093 = CARTESIAN_POINT('Origin',(-3.,-1.8,-15.1)) ;
#24094 = CARTESIAN_POINT('',(-3.85,-1.8,-11.3)) ;
#24095 = CARTESIAN_POINT('',(-3.85,-1.8,-13.2)) ;
#24096 = CARTESIAN_POINT('Origin',(-3.,-1.8,-11.3)) ;
#24097 = CARTESIAN_POINT('Origin',(-3.,-1.8,-13.2)) ;
#24098 = CARTESIAN_POINT('',(-4.09,-1.8,-11.3)) ;
#24099 = CARTESIAN_POINT('Origin',(-3.,-1.8,-11.3)) ;
#24100 = CARTESIAN_POINT('',(-4.09,-1.8,-15.1)) ;
#24101 = CARTESIAN_POINT('',(-4.09,-1.8,-13.2)) ;
#24102 = CARTESIAN_POINT('Origin',(-3.,-1.8,-15.1)) ;
#24103 = CARTESIAN_POINT('Origin',(-3.,-1.8,-15.1)) ;
#24104 = CARTESIAN_POINT('Origin',(-3.,-1.8,-11.3)) ;
#24105 = CARTESIAN_POINT('',(0.,0.,0.)) ;
#24106 = CARTESIAN_POINT('Origin',(-29.75,0.109188309203678,-18.4091883092037)) ;
#24107 = CARTESIAN_POINT('',(-30.,0.109188309203678,-18.0591883092037)) ;
#24108 = CARTESIAN_POINT('Origin',(-30.,0.109188309203678,-18.4091883092037)) ;
#24109 = CARTESIAN_POINT('',(-29.5,0.109188309203678,-18.0591883092037)) ;
#24110 = CARTESIAN_POINT('',(-29.75,0.109188309203678,-18.0591883092037)) ;
#24111 = CARTESIAN_POINT('Origin',(-29.5,0.109188309203678,-18.4091883092037)) ;
#24112 = CARTESIAN_POINT('Origin',(-29.75,-3.70918830920368,-18.4091883092037)) ;
#24113 = CARTESIAN_POINT('',(-30.,-3.70918830920368,-18.0591883092037)) ;
#24114 = CARTESIAN_POINT('Origin',(-30.,-3.70918830920368,-18.4091883092037)) ;
#24115 = CARTESIAN_POINT('',(-29.5,-3.70918830920368,-18.0591883092037)) ;
#24116 = CARTESIAN_POINT('',(-29.75,-3.70918830920368,-18.0591883092037)) ;
#24117 = CARTESIAN_POINT('Origin',(-29.5,-3.70918830920368,-18.4091883092037)) ;
#24118 = CARTESIAN_POINT('Origin',(-29.75,-3.70918830920368,-14.5908116907963)) ;
#24119 = CARTESIAN_POINT('',(-30.,-3.70918830920368,-14.2408116907963)) ;
#24120 = CARTESIAN_POINT('Origin',(-30.,-3.70918830920368,-14.5908116907963)) ;
#24121 = CARTESIAN_POINT('',(-29.5,-3.70918830920368,-14.2408116907963)) ;
#24122 = CARTESIAN_POINT('',(-29.75,-3.70918830920368,-14.2408116907963)) ;
#24123 = CARTESIAN_POINT('Origin',(-29.5,-3.70918830920368,-14.5908116907963)) ;
#24124 = CARTESIAN_POINT('Origin',(-29.75,0.109188309203678,-14.5908116907963)) ;
#24125 = CARTESIAN_POINT('',(-30.,0.109188309203678,-14.2408116907963)) ;
#24126 = CARTESIAN_POINT('Origin',(-30.,0.109188309203678,-14.5908116907963)) ;
#24127 = CARTESIAN_POINT('',(-29.5,0.109188309203679,-14.2408116907963)) ;
#24128 = CARTESIAN_POINT('',(-29.75,0.109188309203678,-14.2408116907963)) ;
#24129 = CARTESIAN_POINT('Origin',(-29.5,0.109188309203678,-14.5908116907963)) ;
#24130 = CARTESIAN_POINT('Origin',(-29.75,-1.8,-16.5)) ;
#24131 = CARTESIAN_POINT('',(-30.,-1.8,-14.75)) ;
#24132 = CARTESIAN_POINT('Origin',(-30.,-1.8,-16.5)) ;
#24133 = CARTESIAN_POINT('',(-29.5,-1.8,-14.75)) ;
#24134 = CARTESIAN_POINT('',(-29.75,-1.8,-14.75)) ;
#24135 = CARTESIAN_POINT('Origin',(-29.5,-1.8,-16.5)) ;
#24136 = CARTESIAN_POINT('Origin',(-29.75,-1.8,-16.5)) ;
#24137 = CARTESIAN_POINT('',(-29.5,-1.8,-13.)) ;
#24138 = CARTESIAN_POINT('Origin',(-29.5,-1.8,-16.5)) ;
#24139 = CARTESIAN_POINT('',(-30.,-1.8,-13.)) ;
#24140 = CARTESIAN_POINT('',(-29.75,-1.8,-13.)) ;
#24141 = CARTESIAN_POINT('Origin',(-30.,-1.8,-16.5)) ;
#24142 = CARTESIAN_POINT('Origin',(-30.,-1.8,-16.5)) ;
#24143 = CARTESIAN_POINT('Origin',(-29.5,-1.8,-16.5)) ;
#24144 = CARTESIAN_POINT('',(0.,0.,0.)) ;
#24145 = CARTESIAN_POINT('Origin',(7.75,0.109188309203678,-18.4091883092037)) ;
#24146 = CARTESIAN_POINT('',(7.5,0.109188309203678,-18.0591883092037)) ;
#24147 = CARTESIAN_POINT('Origin',(7.5,0.109188309203678,-18.4091883092037)) ;
#24148 = CARTESIAN_POINT('',(8.,0.109188309203678,-18.0591883092037)) ;
#24149 = CARTESIAN_POINT('',(7.75,0.109188309203678,-18.0591883092037)) ;
#24150 = CARTESIAN_POINT('Origin',(8.,0.109188309203678,-18.4091883092037)) ;
#24151 = CARTESIAN_POINT('Origin',(7.75,-3.70918830920368,-18.4091883092037)) ;
#24152 = CARTESIAN_POINT('',(7.5,-3.70918830920368,-18.0591883092037)) ;
#24153 = CARTESIAN_POINT('Origin',(7.5,-3.70918830920368,-18.4091883092037)) ;
#24154 = CARTESIAN_POINT('',(8.,-3.70918830920368,-18.0591883092037)) ;
#24155 = CARTESIAN_POINT('',(7.75,-3.70918830920368,-18.0591883092037)) ;
#24156 = CARTESIAN_POINT('Origin',(8.,-3.70918830920368,-18.4091883092037)) ;
#24157 = CARTESIAN_POINT('Origin',(7.75,-3.70918830920368,-14.5908116907963)) ;
#24158 = CARTESIAN_POINT('',(7.5,-3.70918830920368,-14.2408116907963)) ;
#24159 = CARTESIAN_POINT('Origin',(7.5,-3.70918830920368,-14.5908116907963)) ;
#24160 = CARTESIAN_POINT('',(8.,-3.70918830920368,-14.2408116907963)) ;
#24161 = CARTESIAN_POINT('',(7.75,-3.70918830920368,-14.2408116907963)) ;
#24162 = CARTESIAN_POINT('Origin',(8.,-3.70918830920368,-14.5908116907963)) ;
#24163 = CARTESIAN_POINT('Origin',(7.75,0.109188309203678,-14.5908116907963)) ;
#24164 = CARTESIAN_POINT('',(7.5,0.109188309203678,-14.2408116907963)) ;
#24165 = CARTESIAN_POINT('Origin',(7.5,0.109188309203678,-14.5908116907963)) ;
#24166 = CARTESIAN_POINT('',(8.,0.109188309203679,-14.2408116907963)) ;
#24167 = CARTESIAN_POINT('',(7.75,0.109188309203678,-14.2408116907963)) ;
#24168 = CARTESIAN_POINT('Origin',(8.,0.109188309203678,-14.5908116907963)) ;
#24169 = CARTESIAN_POINT('Origin',(7.75,-1.8,-16.5)) ;
#24170 = CARTESIAN_POINT('',(7.5,-1.8,-14.75)) ;
#24171 = CARTESIAN_POINT('Origin',(7.5,-1.8,-16.5)) ;
#24172 = CARTESIAN_POINT('',(8.,-1.8,-14.75)) ;
#24173 = CARTESIAN_POINT('',(7.75,-1.8,-14.75)) ;
#24174 = CARTESIAN_POINT('Origin',(8.,-1.8,-16.5)) ;
#24175 = CARTESIAN_POINT('Origin',(7.75,-1.8,-16.5)) ;
#24176 = CARTESIAN_POINT('',(8.,-1.8,-13.)) ;
#24177 = CARTESIAN_POINT('Origin',(8.,-1.8,-16.5)) ;
#24178 = CARTESIAN_POINT('',(7.5,-1.8,-13.)) ;
#24179 = CARTESIAN_POINT('',(7.75,-1.8,-13.)) ;
#24180 = CARTESIAN_POINT('Origin',(7.5,-1.8,-16.5)) ;
#24181 = CARTESIAN_POINT('Origin',(7.5,-1.8,-16.5)) ;
#24182 = CARTESIAN_POINT('Origin',(8.,-1.8,-16.5)) ;
#24183 = CARTESIAN_POINT('',(0.,0.,0.)) ;
#24184 = CARTESIAN_POINT('Origin',(0.,-1.,-18.4)) ;
#24185 = CARTESIAN_POINT('',(0.32358823443885,-1.03025978408297,-18.4)) ;
#24186 = CARTESIAN_POINT('',(-0.32358823443885,-1.03025978408297,-18.4)) ;
#24187 = CARTESIAN_POINT('',(0.,-1.03025978408297,-18.4)) ;
#24188 = CARTESIAN_POINT('Origin',(0.,-1.,-18.4)) ;
#24189 = CARTESIAN_POINT('Origin',(0.,-1.,-19.1)) ;
#24190 = CARTESIAN_POINT('',(-0.325,-1.,-19.7)) ;
#24191 = CARTESIAN_POINT('Origin',(0.,-1.,-19.7)) ;
#24192 = CARTESIAN_POINT('',(-0.325,-1.,-18.5)) ;
#24193 = CARTESIAN_POINT('',(-0.325,-1.,-19.1)) ;
#24194 = CARTESIAN_POINT('Origin',(0.,-1.,-18.5)) ;
#24195 = CARTESIAN_POINT('Origin',(0.,-1.,-19.1)) ;
#24196 = CARTESIAN_POINT('Ctrl Pts',(-0.32358823443885,-1.03025978408297,
-18.4)) ;
#24197 = CARTESIAN_POINT('Ctrl Pts',(-0.320683284716929,-1.06132436633751,
-18.4125850832905)) ;
#24198 = CARTESIAN_POINT('Ctrl Pts',(-0.313012256587164,-1.093473322376,-18.4246724562692)) ;
#24199 = CARTESIAN_POINT('Ctrl Pts',(-0.283688317673296,-1.16453182056614,
-18.4494936673328)) ;
#24200 = CARTESIAN_POINT('Ctrl Pts',(-0.258016677129131,-1.20214547201537,
-18.4611303131333)) ;
#24201 = CARTESIAN_POINT('Ctrl Pts',(-0.199245732245778,-1.25982709091893,
-18.4777651627884)) ;
#24202 = CARTESIAN_POINT('Ctrl Pts',(-0.16316880358915,-1.28432292672745,
-18.4841520686026)) ;
#24203 = CARTESIAN_POINT('Ctrl Pts',(-0.0838450021535121,-1.31691261760816,
-18.4923375343137)) ;
#24204 = CARTESIAN_POINT('Ctrl Pts',(-0.0406031522762289,-1.325,-18.4942103700463)) ;
#24205 = CARTESIAN_POINT('Ctrl Pts',(0.,-1.325,-18.4942103700463)) ;
#24206 = CARTESIAN_POINT('Ctrl Pts',(0.0406031522762288,-1.325,-18.4942103700463)) ;
#24207 = CARTESIAN_POINT('Ctrl Pts',(0.083845002153512,-1.31691261760816,
-18.4923375343137)) ;
#24208 = CARTESIAN_POINT('Ctrl Pts',(0.16316880358915,-1.28432292672745,-18.4841520686026)) ;
#24209 = CARTESIAN_POINT('Ctrl Pts',(0.199245732245778,-1.25982709091893,
-18.4777651627884)) ;
#24210 = CARTESIAN_POINT('Ctrl Pts',(0.258016677129131,-1.20214547201537,
-18.4611303131333)) ;
#24211 = CARTESIAN_POINT('Ctrl Pts',(0.283688317673296,-1.16453182056614,
-18.4494936673328)) ;
#24212 = CARTESIAN_POINT('Ctrl Pts',(0.313012256587164,-1.093473322376,-18.4246724562692)) ;
#24213 = CARTESIAN_POINT('Ctrl Pts',(0.320683284716929,-1.06132436633751,
-18.4125850832905)) ;
#24214 = CARTESIAN_POINT('Ctrl Pts',(0.32358823443885,-1.03025978408297,-18.4)) ;
#24215 = CARTESIAN_POINT('Origin',(0.,-2.6,-18.4)) ;
#24216 = CARTESIAN_POINT('',(-0.32358823443885,-2.56974021591703,-18.4)) ;
#24217 = CARTESIAN_POINT('',(0.32358823443885,-2.56974021591703,-18.4)) ;
#24218 = CARTESIAN_POINT('',(0.,-2.56974021591703,-18.4)) ;
#24219 = CARTESIAN_POINT('Origin',(0.,-2.6,-18.4)) ;
#24220 = CARTESIAN_POINT('Origin',(0.,-2.6,-19.1)) ;
#24221 = CARTESIAN_POINT('',(-0.325,-2.6,-19.7)) ;
#24222 = CARTESIAN_POINT('Origin',(0.,-2.6,-19.7)) ;
#24223 = CARTESIAN_POINT('',(-0.325,-2.6,-18.5)) ;
#24224 = CARTESIAN_POINT('',(-0.325,-2.6,-19.1)) ;
#24225 = CARTESIAN_POINT('Origin',(0.,-2.6,-18.5)) ;
#24226 = CARTESIAN_POINT('Origin',(0.,-2.6,-19.1)) ;
#24227 = CARTESIAN_POINT('Ctrl Pts',(0.32358823443885,-2.56974021591703,-18.4)) ;
#24228 = CARTESIAN_POINT('Ctrl Pts',(0.320683284716929,-2.53867563366249,
-18.4125850832905)) ;
#24229 = CARTESIAN_POINT('Ctrl Pts',(0.313012256587164,-2.506526677624,-18.4246724562692)) ;
#24230 = CARTESIAN_POINT('Ctrl Pts',(0.283688317673296,-2.43546817943386,
-18.4494936673328)) ;
#24231 = CARTESIAN_POINT('Ctrl Pts',(0.258016677129131,-2.39785452798463,
-18.4611303131333)) ;
#24232 = CARTESIAN_POINT('Ctrl Pts',(0.199245732245778,-2.34017290908107,
-18.4777651627884)) ;
#24233 = CARTESIAN_POINT('Ctrl Pts',(0.16316880358915,-2.31567707327255,-18.4841520686026)) ;
#24234 = CARTESIAN_POINT('Ctrl Pts',(0.0838450021535119,-2.28308738239184,
-18.4923375343137)) ;
#24235 = CARTESIAN_POINT('Ctrl Pts',(0.0406031522762289,-2.275,-18.4942103700463)) ;
#24236 = CARTESIAN_POINT('Ctrl Pts',(-0.0406031522762288,-2.275,-18.4942103700463)) ;
#24237 = CARTESIAN_POINT('Ctrl Pts',(-0.0838450021535119,-2.28308738239184,
-18.4923375343137)) ;
#24238 = CARTESIAN_POINT('Ctrl Pts',(-0.16316880358915,-2.31567707327255,
-18.4841520686026)) ;
#24239 = CARTESIAN_POINT('Ctrl Pts',(-0.199245732245778,-2.34017290908107,
-18.4777651627884)) ;
#24240 = CARTESIAN_POINT('Ctrl Pts',(-0.258016677129131,-2.39785452798463,
-18.4611303131333)) ;
#24241 = CARTESIAN_POINT('Ctrl Pts',(-0.283688317673296,-2.43546817943386,
-18.4494936673328)) ;
#24242 = CARTESIAN_POINT('Ctrl Pts',(-0.313012256587164,-2.506526677624,-18.4246724562692)) ;
#24243 = CARTESIAN_POINT('Ctrl Pts',(-0.320683284716929,-2.53867563366249,
-18.4125850832905)) ;
#24244 = CARTESIAN_POINT('Ctrl Pts',(-0.32358823443885,-2.56974021591703,
-18.4)) ;
#24245 = CARTESIAN_POINT('Origin',(0.,-1.8,-18.5)) ;
#24246 = CARTESIAN_POINT('',(-1.,-2.25,-18.5)) ;
#24247 = CARTESIAN_POINT('',(1.,-2.25,-18.5)) ;
#24248 = CARTESIAN_POINT('',(0.,-2.25,-18.5)) ;
#24249 = CARTESIAN_POINT('',(-1.,-3.3,-18.5)) ;
#24250 = CARTESIAN_POINT('',(-1.,-1.8,-18.5)) ;
#24251 = CARTESIAN_POINT('',(1.,-3.3,-18.5)) ;
#24252 = CARTESIAN_POINT('',(0.,-3.3,-18.5)) ;
#24253 = CARTESIAN_POINT('',(1.,-1.8,-18.5)) ;
#24254 = CARTESIAN_POINT('Origin',(0.,-1.8,-18.5)) ;
#24255 = CARTESIAN_POINT('',(1.,-1.35,-18.5)) ;
#24256 = CARTESIAN_POINT('',(-1.,-1.35,-18.5)) ;
#24257 = CARTESIAN_POINT('',(0.,-1.35,-18.5)) ;
#24258 = CARTESIAN_POINT('',(1.,-0.3,-18.5)) ;
#24259 = CARTESIAN_POINT('',(1.,-1.8,-18.5)) ;
#24260 = CARTESIAN_POINT('',(-1.,-0.3,-18.5)) ;
#24261 = CARTESIAN_POINT('',(0.,-0.3,-18.5)) ;
#24262 = CARTESIAN_POINT('',(-1.,-1.8,-18.5)) ;
#24263 = CARTESIAN_POINT('Origin',(0.,-1.8,-19.7)) ;
#24264 = CARTESIAN_POINT('',(1.,-0.3,-19.7)) ;
#24265 = CARTESIAN_POINT('',(1.,-3.3,-19.7)) ;
#24266 = CARTESIAN_POINT('',(1.,-1.8,-19.7)) ;
#24267 = CARTESIAN_POINT('',(-1.,-3.3,-19.7)) ;
#24268 = CARTESIAN_POINT('',(0.,-3.3,-19.7)) ;
#24269 = CARTESIAN_POINT('',(-1.,-0.3,-19.7)) ;
#24270 = CARTESIAN_POINT('',(-1.,-1.8,-19.7)) ;
#24271 = CARTESIAN_POINT('',(0.,-0.3,-19.7)) ;
#24272 = CARTESIAN_POINT('Origin',(0.,-3.3,-19.1)) ;
#24273 = CARTESIAN_POINT('',(-1.,-3.3,-19.1)) ;
#24274 = CARTESIAN_POINT('',(1.,-3.3,-19.1)) ;
#24275 = CARTESIAN_POINT('Origin',(0.,-0.3,-19.1)) ;
#24276 = CARTESIAN_POINT('',(1.,-0.3,-19.1)) ;
#24277 = CARTESIAN_POINT('',(-1.,-0.3,-19.1)) ;
#24278 = CARTESIAN_POINT('Origin',(-1.,-1.8,-16.5)) ;
#24279 = CARTESIAN_POINT('Origin',(-1.,-1.8,-16.5)) ;
#24280 = CARTESIAN_POINT('',(-1.,-1.8,-14.75)) ;
#24281 = CARTESIAN_POINT('Origin',(-1.,-1.8,-16.5)) ;
#24282 = CARTESIAN_POINT('Origin',(0.,-1.8,-16.5)) ;
#24283 = CARTESIAN_POINT('Origin',(1.,-1.8,-16.5)) ;
#24284 = CARTESIAN_POINT('Origin',(0.,-1.8,-16.5)) ;
#24285 = CARTESIAN_POINT('',(1.,-1.8,-14.75)) ;
#24286 = CARTESIAN_POINT('',(0.,-1.8,-14.75)) ;
#24287 = CARTESIAN_POINT('Origin',(1.,-1.8,-16.5)) ;
#24288 = CARTESIAN_POINT('Origin',(1.,-1.8,-16.5)) ;
#24289 = CARTESIAN_POINT('',(0.,0.,0.)) ;
#24290 = CARTESIAN_POINT('',(0.,0.,0.)) ;
#24291 = CARTESIAN_POINT('',(0.,0.,0.)) ;
#24292 = CARTESIAN_POINT('',(0.,0.,0.)) ;
#24293 = CARTESIAN_POINT('',(0.,0.,0.)) ;
#24294 = CARTESIAN_POINT('',(-25.,0.,0.)) ;
#24295 = CARTESIAN_POINT('',(4.,0.,0.)) ;
#24296 = CARTESIAN_POINT('',(0.,0.,0.)) ;
#24297 = CARTESIAN_POINT('',(0.,0.,0.)) ;
#24298 = CARTESIAN_POINT('Origin',(0.,-0.6,0.)) ;
#24299 = CARTESIAN_POINT('',(-0.195,-1.2,-2.38806125833734E-17)) ;
#24300 = CARTESIAN_POINT('Origin',(0.,-1.2,0.)) ;
#24301 = CARTESIAN_POINT('',(-0.195,0.,-2.38806125833734E-17)) ;
#24302 = CARTESIAN_POINT('',(-0.195,-0.6,-2.38806125833734E-17)) ;
#24303 = CARTESIAN_POINT('Origin',(0.,0.,0.)) ;
#24304 = CARTESIAN_POINT('Origin',(0.,-1.2,0.)) ;
#24305 = CARTESIAN_POINT('Origin',(0.,0.125,0.)) ;
#24306 = CARTESIAN_POINT('',(-0.35,0.,-4.28626379701574E-17)) ;
#24307 = CARTESIAN_POINT('Origin',(0.,0.,0.)) ;
#24308 = CARTESIAN_POINT('',(-0.35,0.25,-4.28626379701574E-17)) ;
#24309 = CARTESIAN_POINT('',(-0.35,0.125,-4.28626379701574E-17)) ;
#24310 = CARTESIAN_POINT('Origin',(0.,0.25,0.)) ;
#24311 = CARTESIAN_POINT('Origin',(0.,0.25,0.)) ;
#24312 = CARTESIAN_POINT('Origin',(0.,0.,0.)) ;
#24313 = CARTESIAN_POINT('',(0.,0.,0.)) ;
#24314 = CARTESIAN_POINT('Origin',(0.,-0.2,0.)) ;
#24315 = CARTESIAN_POINT('',(-0.525,-0.3,6.4293956955236E-17)) ;
#24316 = CARTESIAN_POINT('Origin',(0.,-0.3,0.)) ;
#24317 = CARTESIAN_POINT('',(-0.525,-0.1,-6.4293956955236E-17)) ;
#24318 = CARTESIAN_POINT('',(-0.525,-0.2,6.4293956955236E-17)) ;
#24319 = CARTESIAN_POINT('Origin',(0.,-0.1,0.)) ;
#24320 = CARTESIAN_POINT('Origin',(0.,-0.2,0.)) ;
#24321 = CARTESIAN_POINT('',(-1.,-0.1,1.22464679914735E-16)) ;
#24322 = CARTESIAN_POINT('Origin',(0.,-0.1,0.)) ;
#24323 = CARTESIAN_POINT('',(-1.,-0.3,1.22464679914735E-16)) ;
#24324 = CARTESIAN_POINT('',(-1.,-0.2,1.22464679914735E-16)) ;
#24325 = CARTESIAN_POINT('Origin',(0.,-0.3,0.)) ;
#24326 = CARTESIAN_POINT('Origin',(0.,-0.3,0.)) ;
#24327 = CARTESIAN_POINT('Origin',(0.,-0.1,0.)) ;
#24328 = CARTESIAN_POINT('',(0.,0.,0.)) ;
#24329 = CARTESIAN_POINT('Origin',(0.,0.3,0.)) ;
#24330 = CARTESIAN_POINT('',(-0.5,-0.1,6.12323399573677E-17)) ;
#24331 = CARTESIAN_POINT('Origin',(0.,-0.1,0.)) ;
#24332 = CARTESIAN_POINT('',(-0.5,0.7,-6.12323399573677E-17)) ;
#24333 = CARTESIAN_POINT('',(-0.5,0.3,6.12323399573677E-17)) ;
#24334 = CARTESIAN_POINT('Origin',(0.,0.7,0.)) ;
#24335 = CARTESIAN_POINT('Origin',(0.425,0.3,0.736121593216773)) ;
#24336 = CARTESIAN_POINT('',(-3.33066907387547E-16,-0.1,0.981495457622364)) ;
#24337 = CARTESIAN_POINT('',(-3.33066907387547E-16,0.7,0.981495457622364)) ;
#24338 = CARTESIAN_POINT('',(-3.33066907387547E-16,0.3,0.981495457622364)) ;
#24339 = CARTESIAN_POINT('',(0.85,-0.1,0.490747728811182)) ;
#24340 = CARTESIAN_POINT('',(0.425,-0.1,0.736121593216773)) ;
#24341 = CARTESIAN_POINT('',(0.85,0.7,0.490747728811182)) ;
#24342 = CARTESIAN_POINT('',(0.85,0.3,0.490747728811182)) ;
#24343 = CARTESIAN_POINT('',(0.425,0.7,0.736121593216773)) ;
#24344 = CARTESIAN_POINT('Origin',(-0.425,0.3,-0.736121593216773)) ;
#24345 = CARTESIAN_POINT('',(3.33066907387547E-16,-0.1,-0.981495457622364)) ;
#24346 = CARTESIAN_POINT('',(3.33066907387547E-16,0.7,-0.981495457622364)) ;
#24347 = CARTESIAN_POINT('',(3.33066907387547E-16,0.3,-0.981495457622364)) ;
#24348 = CARTESIAN_POINT('',(-0.85,-0.1,-0.490747728811182)) ;
#24349 = CARTESIAN_POINT('',(-0.425,-0.1,-0.736121593216773)) ;
#24350 = CARTESIAN_POINT('',(-0.85,0.7,-0.490747728811182)) ;
#24351 = CARTESIAN_POINT('',(-0.85,0.3,-0.490747728811182)) ;
#24352 = CARTESIAN_POINT('',(-0.425,0.7,-0.736121593216773)) ;
#24353 = CARTESIAN_POINT('Origin',(0.,-0.1,0.)) ;
#24354 = CARTESIAN_POINT('',(-0.85,-0.1,0.490747728811182)) ;
#24355 = CARTESIAN_POINT('',(-0.425,-0.1,0.736121593216773)) ;
#24356 = CARTESIAN_POINT('',(-0.85,-0.1,0.)) ;
#24357 = CARTESIAN_POINT('',(0.85,-0.1,-0.490747728811182)) ;
#24358 = CARTESIAN_POINT('',(0.425,-0.1,-0.736121593216773)) ;
#24359 = CARTESIAN_POINT('',(0.85,-0.1,0.)) ;
#24360 = CARTESIAN_POINT('Origin',(-0.425,0.3,0.736121593216773)) ;
#24361 = CARTESIAN_POINT('',(-0.85,0.7,0.490747728811182)) ;
#24362 = CARTESIAN_POINT('',(-0.85,0.3,0.490747728811182)) ;
#24363 = CARTESIAN_POINT('',(-0.425,0.7,0.736121593216773)) ;
#24364 = CARTESIAN_POINT('Origin',(0.425,0.3,-0.736121593216773)) ;
#24365 = CARTESIAN_POINT('',(0.85,0.7,-0.490747728811182)) ;
#24366 = CARTESIAN_POINT('',(0.85,0.3,-0.490747728811182)) ;
#24367 = CARTESIAN_POINT('',(0.425,0.7,-0.736121593216773)) ;
#24368 = CARTESIAN_POINT('Origin',(-0.85,0.3,0.)) ;
#24369 = CARTESIAN_POINT('',(-0.85,0.7,0.)) ;
#24370 = CARTESIAN_POINT('Origin',(0.85,0.3,0.)) ;
#24371 = CARTESIAN_POINT('',(0.85,0.7,0.)) ;
#24372 = CARTESIAN_POINT('Origin',(0.,0.7,0.)) ;
#24373 = CARTESIAN_POINT('',(0.,0.,0.)) ;
#24374 = CARTESIAN_POINT('Origin',(0.,0.8,0.)) ;
#24375 = CARTESIAN_POINT('',(-0.4,1.6,4.89858719658941E-17)) ;
#24376 = CARTESIAN_POINT('Origin',(0.,1.6,0.)) ;
#24377 = CARTESIAN_POINT('',(-0.4,0.,4.89858719658941E-17)) ;
#24378 = CARTESIAN_POINT('',(-0.4,0.8,4.89858719658941E-17)) ;
#24379 = CARTESIAN_POINT('Origin',(0.,0.,0.)) ;
#24380 = CARTESIAN_POINT('Origin',(0.,1.6,0.)) ;
#24381 = CARTESIAN_POINT('Origin',(0.325,-0.265,0.562916512459885)) ;
#24382 = CARTESIAN_POINT('',(0.,-0.53,0.750555349946514)) ;
#24383 = CARTESIAN_POINT('',(0.,0.,0.750555349946514)) ;
#24384 = CARTESIAN_POINT('',(0.,-0.265,0.750555349946514)) ;
#24385 = CARTESIAN_POINT('',(0.65,-0.53,0.375277674973257)) ;
#24386 = CARTESIAN_POINT('',(0.325,-0.53,0.562916512459885)) ;
#24387 = CARTESIAN_POINT('',(0.65,0.,0.375277674973257)) ;
#24388 = CARTESIAN_POINT('',(0.65,-0.265,0.375277674973257)) ;
#24389 = CARTESIAN_POINT('',(0.325,0.,0.562916512459885)) ;
#24390 = CARTESIAN_POINT('Origin',(-0.325,-0.265,-0.562916512459885)) ;
#24391 = CARTESIAN_POINT('',(0.,-0.53,-0.750555349946514)) ;
#24392 = CARTESIAN_POINT('',(0.,0.,-0.750555349946514)) ;
#24393 = CARTESIAN_POINT('',(0.,-0.265,-0.750555349946514)) ;
#24394 = CARTESIAN_POINT('',(-0.65,-0.53,-0.375277674973257)) ;
#24395 = CARTESIAN_POINT('',(-0.325,-0.53,-0.562916512459885)) ;
#24396 = CARTESIAN_POINT('',(-0.65,0.,-0.375277674973257)) ;
#24397 = CARTESIAN_POINT('',(-0.65,-0.265,-0.375277674973257)) ;
#24398 = CARTESIAN_POINT('',(-0.325,0.,-0.562916512459885)) ;
#24399 = CARTESIAN_POINT('Origin',(0.,-0.53,0.)) ;
#24400 = CARTESIAN_POINT('',(-0.65,-0.53,0.375277674973257)) ;
#24401 = CARTESIAN_POINT('',(-0.325,-0.53,0.562916512459885)) ;
#24402 = CARTESIAN_POINT('',(-0.65,-0.53,0.)) ;
#24403 = CARTESIAN_POINT('',(0.65,-0.53,-0.375277674973257)) ;
#24404 = CARTESIAN_POINT('',(0.325,-0.53,-0.562916512459885)) ;
#24405 = CARTESIAN_POINT('',(0.65,-0.53,0.)) ;
#24406 = CARTESIAN_POINT('Origin',(-0.325,-0.265,0.562916512459885)) ;
#24407 = CARTESIAN_POINT('',(-0.65,0.,0.375277674973257)) ;
#24408 = CARTESIAN_POINT('',(-0.65,-0.265,0.375277674973257)) ;
#24409 = CARTESIAN_POINT('',(-0.325,0.,0.562916512459885)) ;
#24410 = CARTESIAN_POINT('Origin',(0.325,-0.265,-0.562916512459885)) ;
#24411 = CARTESIAN_POINT('',(0.65,0.,-0.375277674973257)) ;
#24412 = CARTESIAN_POINT('',(0.65,-0.265,-0.375277674973257)) ;
#24413 = CARTESIAN_POINT('',(0.325,0.,-0.562916512459885)) ;
#24414 = CARTESIAN_POINT('Origin',(-0.65,-0.265,0.)) ;
#24415 = CARTESIAN_POINT('',(-0.65,0.,0.)) ;
#24416 = CARTESIAN_POINT('Origin',(0.65,-0.265,0.)) ;
#24417 = CARTESIAN_POINT('',(0.65,0.,0.)) ;
#24418 = CARTESIAN_POINT('Origin',(0.,0.,0.)) ;
#24419 = CARTESIAN_POINT('',(0.,0.,0.)) ;
#24420 = CARTESIAN_POINT('Origin',(0.,-4.25,0.)) ;
#24421 = CARTESIAN_POINT('',(-0.3,-8.5,-3.67394039744206E-17)) ;
#24422 = CARTESIAN_POINT('Origin',(0.,-8.5,0.)) ;
#24423 = CARTESIAN_POINT('',(-0.3,0.,-3.67394039744206E-17)) ;
#24424 = CARTESIAN_POINT('',(-0.3,-4.25,-3.67394039744206E-17)) ;
#24425 = CARTESIAN_POINT('Origin',(0.,0.,0.)) ;
#24426 = CARTESIAN_POINT('Origin',(0.,-8.5,0.)) ;
#24427 = CARTESIAN_POINT('Origin',(0.25,0.2,-0.433012701892219)) ;
#24428 = CARTESIAN_POINT('',(-8.32667268468867E-17,0.4,-0.577350269189626)) ;
#24429 = CARTESIAN_POINT('',(-8.32667268468867E-17,0.,-0.577350269189626)) ;
#24430 = CARTESIAN_POINT('',(-8.32667268468867E-17,0.2,-0.577350269189626)) ;
#24431 = CARTESIAN_POINT('',(0.5,0.4,-0.288675134594813)) ;
#24432 = CARTESIAN_POINT('',(0.25,0.4,-0.433012701892219)) ;
#24433 = CARTESIAN_POINT('',(0.5,0.,-0.288675134594813)) ;
#24434 = CARTESIAN_POINT('',(0.5,0.2,-0.288675134594813)) ;
#24435 = CARTESIAN_POINT('',(0.25,0.,-0.433012701892219)) ;
#24436 = CARTESIAN_POINT('Origin',(-0.25,0.2,0.433012701892219)) ;
#24437 = CARTESIAN_POINT('',(8.32667268468867E-17,0.4,0.577350269189626)) ;
#24438 = CARTESIAN_POINT('',(8.32667268468867E-17,0.,0.577350269189626)) ;
#24439 = CARTESIAN_POINT('',(8.32667268468867E-17,0.2,0.577350269189626)) ;
#24440 = CARTESIAN_POINT('',(-0.5,0.4,0.288675134594813)) ;
#24441 = CARTESIAN_POINT('',(-0.25,0.4,0.433012701892219)) ;
#24442 = CARTESIAN_POINT('',(-0.5,0.,0.288675134594813)) ;
#24443 = CARTESIAN_POINT('',(-0.5,0.2,0.288675134594813)) ;
#24444 = CARTESIAN_POINT('',(-0.25,0.,0.433012701892219)) ;
#24445 = CARTESIAN_POINT('Origin',(0.,0.4,0.)) ;
#24446 = CARTESIAN_POINT('',(-0.5,0.4,-0.288675134594813)) ;
#24447 = CARTESIAN_POINT('',(-0.25,0.4,-0.433012701892219)) ;
#24448 = CARTESIAN_POINT('',(-0.5,0.4,0.)) ;
#24449 = CARTESIAN_POINT('',(0.5,0.4,0.288675134594813)) ;
#24450 = CARTESIAN_POINT('',(0.25,0.4,0.433012701892219)) ;
#24451 = CARTESIAN_POINT('',(0.5,0.4,0.)) ;
#24452 = CARTESIAN_POINT('Origin',(-0.25,0.2,-0.433012701892219)) ;
#24453 = CARTESIAN_POINT('',(-0.5,0.,-0.288675134594813)) ;
#24454 = CARTESIAN_POINT('',(-0.5,0.2,-0.288675134594813)) ;
#24455 = CARTESIAN_POINT('',(-0.25,0.,-0.433012701892219)) ;
#24456 = CARTESIAN_POINT('Origin',(0.25,0.2,0.433012701892219)) ;
#24457 = CARTESIAN_POINT('',(0.5,0.,0.288675134594813)) ;
#24458 = CARTESIAN_POINT('',(0.5,0.2,0.288675134594813)) ;
#24459 = CARTESIAN_POINT('',(0.25,0.,0.433012701892219)) ;
#24460 = CARTESIAN_POINT('Origin',(-0.5,0.2,0.)) ;
#24461 = CARTESIAN_POINT('',(-0.5,0.,0.)) ;
#24462 = CARTESIAN_POINT('Origin',(0.5,0.2,0.)) ;
#24463 = CARTESIAN_POINT('',(0.5,0.,0.)) ;
#24464 = CARTESIAN_POINT('Origin',(0.,0.,0.)) ;
#24465 = CARTESIAN_POINT('',(0.,0.,0.)) ;
#24466 = CARTESIAN_POINT('Origin',(0.,0.,0.)) ;
#24467 = CARTESIAN_POINT('',(-0.3,-0.25,3.67394039744206E-17)) ;
#24468 = CARTESIAN_POINT('Origin',(0.,-0.25,0.)) ;
#24469 = CARTESIAN_POINT('',(-0.3,0.25,-3.67394039744206E-17)) ;
#24470 = CARTESIAN_POINT('',(-0.3,0.,3.67394039744206E-17)) ;
#24471 = CARTESIAN_POINT('Origin',(0.,0.25,0.)) ;
#24472 = CARTESIAN_POINT('Origin',(0.25,0.,0.433012701892219)) ;
#24473 = CARTESIAN_POINT('',(-8.32667268468867E-17,-0.25,0.577350269189626)) ;
#24474 = CARTESIAN_POINT('',(-8.32667268468867E-17,0.25,0.577350269189626)) ;
#24475 = CARTESIAN_POINT('',(-8.32667268468867E-17,0.,0.577350269189626)) ;
#24476 = CARTESIAN_POINT('',(0.5,-0.25,0.288675134594813)) ;
#24477 = CARTESIAN_POINT('',(0.25,-0.25,0.433012701892219)) ;
#24478 = CARTESIAN_POINT('',(0.5,0.25,0.288675134594813)) ;
#24479 = CARTESIAN_POINT('',(0.5,0.,0.288675134594813)) ;
#24480 = CARTESIAN_POINT('',(0.25,0.25,0.433012701892219)) ;
#24481 = CARTESIAN_POINT('Origin',(-0.25,0.,-0.433012701892219)) ;
#24482 = CARTESIAN_POINT('',(8.32667268468867E-17,-0.25,-0.577350269189626)) ;
#24483 = CARTESIAN_POINT('',(8.32667268468867E-17,0.25,-0.577350269189626)) ;
#24484 = CARTESIAN_POINT('',(8.32667268468867E-17,0.,-0.577350269189626)) ;
#24485 = CARTESIAN_POINT('',(-0.5,-0.25,-0.288675134594813)) ;
#24486 = CARTESIAN_POINT('',(-0.25,-0.25,-0.433012701892219)) ;
#24487 = CARTESIAN_POINT('',(-0.5,0.25,-0.288675134594813)) ;
#24488 = CARTESIAN_POINT('',(-0.5,0.,-0.288675134594813)) ;
#24489 = CARTESIAN_POINT('',(-0.25,0.25,-0.433012701892219)) ;
#24490 = CARTESIAN_POINT('Origin',(0.,-0.25,0.)) ;
#24491 = CARTESIAN_POINT('',(-0.5,-0.25,0.288675134594813)) ;
#24492 = CARTESIAN_POINT('',(-0.25,-0.25,0.433012701892219)) ;
#24493 = CARTESIAN_POINT('',(-0.5,-0.25,0.)) ;
#24494 = CARTESIAN_POINT('',(0.5,-0.25,-0.288675134594813)) ;
#24495 = CARTESIAN_POINT('',(0.25,-0.25,-0.433012701892219)) ;
#24496 = CARTESIAN_POINT('',(0.5,-0.25,0.)) ;
#24497 = CARTESIAN_POINT('Origin',(-0.25,0.,0.433012701892219)) ;
#24498 = CARTESIAN_POINT('',(-0.5,0.25,0.288675134594813)) ;
#24499 = CARTESIAN_POINT('',(-0.5,0.,0.288675134594813)) ;
#24500 = CARTESIAN_POINT('',(-0.25,0.25,0.433012701892219)) ;
#24501 = CARTESIAN_POINT('Origin',(0.25,0.,-0.433012701892219)) ;
#24502 = CARTESIAN_POINT('',(0.5,0.25,-0.288675134594813)) ;
#24503 = CARTESIAN_POINT('',(0.5,0.,-0.288675134594813)) ;
#24504 = CARTESIAN_POINT('',(0.25,0.25,-0.433012701892219)) ;
#24505 = CARTESIAN_POINT('Origin',(-0.5,0.,0.)) ;
#24506 = CARTESIAN_POINT('',(-0.5,0.25,0.)) ;
#24507 = CARTESIAN_POINT('Origin',(0.5,0.,0.)) ;
#24508 = CARTESIAN_POINT('',(0.5,0.25,0.)) ;
#24509 = CARTESIAN_POINT('Origin',(0.,0.25,0.)) ;
#24510 = CARTESIAN_POINT('',(1.10218211923262E-16,-0.3,1.8)) ;
#24511 = CARTESIAN_POINT('',(-1.55884572681199,-0.3,-0.9)) ;
#24512 = CARTESIAN_POINT('',(1.55884572681199,-0.3,-0.900000000000001)) ;
#24513 = CARTESIAN_POINT('',(0.,0.,0.)) ;
#24514 = CARTESIAN_POINT('',(0.,0.,0.)) ;
#24515 = CARTESIAN_POINT('',(-2.5,-5.2,11.5)) ;
#24516 = CARTESIAN_POINT('',(2.5,-5.2,11.5)) ;
#24517 = CARTESIAN_POINT('',(11.95,4.,0.)) ;
#24518 = CARTESIAN_POINT('',(11.95,-4.25,0.)) ;
#24519 = CARTESIAN_POINT('',(5.975,4.,10.349003575224)) ;
#24520 = CARTESIAN_POINT('',(5.975,-4.25,10.349003575224)) ;
#24521 = CARTESIAN_POINT('',(-5.975,4.,10.349003575224)) ;
#24522 = CARTESIAN_POINT('',(-5.975,-4.25,10.349003575224)) ;
#24523 = CARTESIAN_POINT('',(-11.95,4.,1.46345292498109E-15)) ;
#24524 = CARTESIAN_POINT('',(-11.95,-4.25,1.46345292498109E-15)) ;
#24525 = CARTESIAN_POINT('',(-5.975,4.,-10.349003575224)) ;
#24526 = CARTESIAN_POINT('',(-5.975,-4.25,-10.349003575224)) ;
#24527 = CARTESIAN_POINT('',(5.975,4.,-10.349003575224)) ;
#24528 = CARTESIAN_POINT('',(5.975,-4.25,-10.349003575224)) ;
#24529 = CARTESIAN_POINT('',(0.,0.,0.)) ;
#24530 = CARTESIAN_POINT('',(0.,0.,0.)) ;
#24531 = CARTESIAN_POINT('',(0.,0.,0.)) ;
#24532 = CARTESIAN_POINT('',(0.,0.,0.)) ;
#24533 = UNCERTAINTY_MEASURE_WITH_UNIT(LENGTH_MEASURE(0.001),#24629,
'DISTANCE_ACCURACY_VALUE',
'Maximum model space distance between geometric entities at asserted c
onnectivities') ;
#24534 = UNCERTAINTY_MEASURE_WITH_UNIT(LENGTH_MEASURE(0.001),#24629,
'DISTANCE_ACCURACY_VALUE',
'Maximum model space distance between geometric entities at asserted c
onnectivities') ;
#24535 = UNCERTAINTY_MEASURE_WITH_UNIT(LENGTH_MEASURE(0.001),#24629,
'DISTANCE_ACCURACY_VALUE',
'Maximum model space distance between geometric entities at asserted c
onnectivities') ;
#24536 = UNCERTAINTY_MEASURE_WITH_UNIT(LENGTH_MEASURE(0.001),#24629,
'DISTANCE_ACCURACY_VALUE',
'Maximum model space distance between geometric entities at asserted c
onnectivities') ;
#24537 = UNCERTAINTY_MEASURE_WITH_UNIT(LENGTH_MEASURE(0.001),#24629,
'DISTANCE_ACCURACY_VALUE',
'Maximum model space distance between geometric entities at asserted c
onnectivities') ;
#24538 = UNCERTAINTY_MEASURE_WITH_UNIT(LENGTH_MEASURE(0.001),#24629,
'DISTANCE_ACCURACY_VALUE',
'Maximum model space distance between geometric entities at asserted c
onnectivities') ;
#24539 = UNCERTAINTY_MEASURE_WITH_UNIT(LENGTH_MEASURE(0.001),#24629,
'DISTANCE_ACCURACY_VALUE',
'Maximum model space distance between geometric entities at asserted c
onnectivities') ;
#24540 = UNCERTAINTY_MEASURE_WITH_UNIT(LENGTH_MEASURE(0.001),#24629,
'DISTANCE_ACCURACY_VALUE',
'Maximum model space distance between geometric entities at asserted c
onnectivities') ;
#24541 = UNCERTAINTY_MEASURE_WITH_UNIT(LENGTH_MEASURE(0.001),#24629,
'DISTANCE_ACCURACY_VALUE',
'Maximum model space distance between geometric entities at asserted c
onnectivities') ;
#24542 = UNCERTAINTY_MEASURE_WITH_UNIT(LENGTH_MEASURE(0.001),#24629,
'DISTANCE_ACCURACY_VALUE',
'Maximum model space distance between geometric entities at asserted c
onnectivities') ;
#24543 = UNCERTAINTY_MEASURE_WITH_UNIT(LENGTH_MEASURE(0.001),#24629,
'DISTANCE_ACCURACY_VALUE',
'Maximum model space distance between geometric entities at asserted c
onnectivities') ;
#24544 = UNCERTAINTY_MEASURE_WITH_UNIT(LENGTH_MEASURE(0.001),#24629,
'DISTANCE_ACCURACY_VALUE',
'Maximum model space distance between geometric entities at asserted c
onnectivities') ;
#24545 = UNCERTAINTY_MEASURE_WITH_UNIT(LENGTH_MEASURE(0.001),#24629,
'DISTANCE_ACCURACY_VALUE',
'Maximum model space distance between geometric entities at asserted c
onnectivities') ;
#24546 = UNCERTAINTY_MEASURE_WITH_UNIT(LENGTH_MEASURE(0.001),#24629,
'DISTANCE_ACCURACY_VALUE',
'Maximum model space distance between geometric entities at asserted c
onnectivities') ;
#24547 = UNCERTAINTY_MEASURE_WITH_UNIT(LENGTH_MEASURE(0.001),#24629,
'DISTANCE_ACCURACY_VALUE',
'Maximum model space distance between geometric entities at asserted c
onnectivities') ;
#24548 = UNCERTAINTY_MEASURE_WITH_UNIT(LENGTH_MEASURE(0.001),#24629,
'DISTANCE_ACCURACY_VALUE',
'Maximum model space distance between geometric entities at asserted c
onnectivities') ;
#24549 = UNCERTAINTY_MEASURE_WITH_UNIT(LENGTH_MEASURE(0.001),#24629,
'DISTANCE_ACCURACY_VALUE',
'Maximum model space distance between geometric entities at asserted c
onnectivities') ;
#24550 = UNCERTAINTY_MEASURE_WITH_UNIT(LENGTH_MEASURE(0.001),#24629,
'DISTANCE_ACCURACY_VALUE',
'Maximum model space distance between geometric entities at asserted c
onnectivities') ;
#24551 = UNCERTAINTY_MEASURE_WITH_UNIT(LENGTH_MEASURE(0.001),#24629,
'DISTANCE_ACCURACY_VALUE',
'Maximum model space distance between geometric entities at asserted c
onnectivities') ;
#24552 = UNCERTAINTY_MEASURE_WITH_UNIT(LENGTH_MEASURE(0.001),#24629,
'DISTANCE_ACCURACY_VALUE',
'Maximum model space distance between geometric entities at asserted c
onnectivities') ;
#24553 = UNCERTAINTY_MEASURE_WITH_UNIT(LENGTH_MEASURE(0.001),#24629,
'DISTANCE_ACCURACY_VALUE',
'Maximum model space distance between geometric entities at asserted c
onnectivities') ;
#24554 = UNCERTAINTY_MEASURE_WITH_UNIT(LENGTH_MEASURE(0.001),#24629,
'DISTANCE_ACCURACY_VALUE',
'Maximum model space distance between geometric entities at asserted c
onnectivities') ;
#24555 = UNCERTAINTY_MEASURE_WITH_UNIT(LENGTH_MEASURE(0.001),#24629,
'DISTANCE_ACCURACY_VALUE',
'Maximum model space distance between geometric entities at asserted c
onnectivities') ;
#24556 = UNCERTAINTY_MEASURE_WITH_UNIT(LENGTH_MEASURE(0.001),#24629,
'DISTANCE_ACCURACY_VALUE',
'Maximum model space distance between geometric entities at asserted c
onnectivities') ;
#24557 = UNCERTAINTY_MEASURE_WITH_UNIT(LENGTH_MEASURE(0.001),#24629,
'DISTANCE_ACCURACY_VALUE',
'Maximum model space distance between geometric entities at asserted c
onnectivities') ;
#24558 = UNCERTAINTY_MEASURE_WITH_UNIT(LENGTH_MEASURE(0.001),#24629,
'DISTANCE_ACCURACY_VALUE',
'Maximum model space distance between geometric entities at asserted c
onnectivities') ;
#24559 = UNCERTAINTY_MEASURE_WITH_UNIT(LENGTH_MEASURE(0.001),#24629,
'DISTANCE_ACCURACY_VALUE',
'Maximum model space distance between geometric entities at asserted c
onnectivities') ;
#24560 = UNCERTAINTY_MEASURE_WITH_UNIT(LENGTH_MEASURE(0.001),#24629,
'DISTANCE_ACCURACY_VALUE',
'Maximum model space distance between geometric entities at asserted c
onnectivities') ;
#24561 = UNCERTAINTY_MEASURE_WITH_UNIT(LENGTH_MEASURE(0.001),#24629,
'DISTANCE_ACCURACY_VALUE',
'Maximum model space distance between geometric entities at asserted c
onnectivities') ;
#24562 = UNCERTAINTY_MEASURE_WITH_UNIT(LENGTH_MEASURE(0.001),#24629,
'DISTANCE_ACCURACY_VALUE',
'Maximum model space distance between geometric entities at asserted c
onnectivities') ;
#24563 = UNCERTAINTY_MEASURE_WITH_UNIT(LENGTH_MEASURE(0.001),#24629,
'DISTANCE_ACCURACY_VALUE',
'Maximum model space distance between geometric entities at asserted c
onnectivities') ;
#24564 = UNCERTAINTY_MEASURE_WITH_UNIT(LENGTH_MEASURE(0.001),#24629,
'DISTANCE_ACCURACY_VALUE',
'Maximum model space distance between geometric entities at asserted c
onnectivities') ;
#24565 = UNCERTAINTY_MEASURE_WITH_UNIT(LENGTH_MEASURE(0.001),#24629,
'DISTANCE_ACCURACY_VALUE',
'Maximum model space distance between geometric entities at asserted c
onnectivities') ;
#24566 = UNCERTAINTY_MEASURE_WITH_UNIT(LENGTH_MEASURE(0.001),#24629,
'DISTANCE_ACCURACY_VALUE',
'Maximum model space distance between geometric entities at asserted c
onnectivities') ;
#24567 = UNCERTAINTY_MEASURE_WITH_UNIT(LENGTH_MEASURE(0.001),#24629,
'DISTANCE_ACCURACY_VALUE',
'Maximum model space distance between geometric entities at asserted c
onnectivities') ;
#24568 = UNCERTAINTY_MEASURE_WITH_UNIT(LENGTH_MEASURE(0.001),#24629,
'DISTANCE_ACCURACY_VALUE',
'Maximum model space distance between geometric entities at asserted c
onnectivities') ;
#24569 = UNCERTAINTY_MEASURE_WITH_UNIT(LENGTH_MEASURE(0.001),#24629,
'DISTANCE_ACCURACY_VALUE',
'Maximum model space distance between geometric entities at asserted c
onnectivities') ;
#24570 = UNCERTAINTY_MEASURE_WITH_UNIT(LENGTH_MEASURE(0.001),#24629,
'DISTANCE_ACCURACY_VALUE',
'Maximum model space distance between geometric entities at asserted c
onnectivities') ;
#24571 = UNCERTAINTY_MEASURE_WITH_UNIT(LENGTH_MEASURE(0.001),#24629,
'DISTANCE_ACCURACY_VALUE',
'Maximum model space distance between geometric entities at asserted c
onnectivities') ;
#24572 = UNCERTAINTY_MEASURE_WITH_UNIT(LENGTH_MEASURE(0.001),#24629,
'DISTANCE_ACCURACY_VALUE',
'Maximum model space distance between geometric entities at asserted c
onnectivities') ;
#24573 = UNCERTAINTY_MEASURE_WITH_UNIT(LENGTH_MEASURE(0.001),#24629,
'DISTANCE_ACCURACY_VALUE',
'Maximum model space distance between geometric entities at asserted c
onnectivities') ;
#24574 = UNCERTAINTY_MEASURE_WITH_UNIT(LENGTH_MEASURE(0.001),#24629,
'DISTANCE_ACCURACY_VALUE',
'Maximum model space distance between geometric entities at asserted c
onnectivities') ;
#24575 = UNCERTAINTY_MEASURE_WITH_UNIT(LENGTH_MEASURE(0.001),#24629,
'DISTANCE_ACCURACY_VALUE',
'Maximum model space distance between geometric entities at asserted c
onnectivities') ;
#24576 = UNCERTAINTY_MEASURE_WITH_UNIT(LENGTH_MEASURE(0.001),#24629,
'DISTANCE_ACCURACY_VALUE',
'Maximum model space distance between geometric entities at asserted c
onnectivities') ;
#24577 = UNCERTAINTY_MEASURE_WITH_UNIT(LENGTH_MEASURE(0.001),#24629,
'DISTANCE_ACCURACY_VALUE',
'Maximum model space distance between geometric entities at asserted c
onnectivities') ;
#24578 = UNCERTAINTY_MEASURE_WITH_UNIT(LENGTH_MEASURE(0.001),#24629,
'DISTANCE_ACCURACY_VALUE',
'Maximum model space distance between geometric entities at asserted c
onnectivities') ;
#24579 = UNCERTAINTY_MEASURE_WITH_UNIT(LENGTH_MEASURE(0.001),#24629,
'DISTANCE_ACCURACY_VALUE',
'Maximum model space distance between geometric entities at asserted c
onnectivities') ;
#24580 = UNCERTAINTY_MEASURE_WITH_UNIT(LENGTH_MEASURE(0.001),#24629,
'DISTANCE_ACCURACY_VALUE',
'Maximum model space distance between geometric entities at asserted c
onnectivities') ;
#24581 = (
GEOMETRIC_REPRESENTATION_CONTEXT(3)
GLOBAL_UNCERTAINTY_ASSIGNED_CONTEXT((#24533))
GLOBAL_UNIT_ASSIGNED_CONTEXT((#24629,#24631,#24632))
REPRESENTATION_CONTEXT('','3D')
) ;
#24582 = (
GEOMETRIC_REPRESENTATION_CONTEXT(3)
GLOBAL_UNCERTAINTY_ASSIGNED_CONTEXT((#24534))
GLOBAL_UNIT_ASSIGNED_CONTEXT((#24629,#24631,#24632))
REPRESENTATION_CONTEXT('','3D')
) ;
#24583 = (
GEOMETRIC_REPRESENTATION_CONTEXT(3)
GLOBAL_UNCERTAINTY_ASSIGNED_CONTEXT((#24535))
GLOBAL_UNIT_ASSIGNED_CONTEXT((#24629,#24631,#24632))
REPRESENTATION_CONTEXT('','3D')
) ;
#24584 = (
GEOMETRIC_REPRESENTATION_CONTEXT(3)
GLOBAL_UNCERTAINTY_ASSIGNED_CONTEXT((#24536))
GLOBAL_UNIT_ASSIGNED_CONTEXT((#24629,#24631,#24632))
REPRESENTATION_CONTEXT('','3D')
) ;
#24585 = (
GEOMETRIC_REPRESENTATION_CONTEXT(3)
GLOBAL_UNCERTAINTY_ASSIGNED_CONTEXT((#24537))
GLOBAL_UNIT_ASSIGNED_CONTEXT((#24629,#24631,#24632))
REPRESENTATION_CONTEXT('','3D')
) ;
#24586 = (
GEOMETRIC_REPRESENTATION_CONTEXT(3)
GLOBAL_UNCERTAINTY_ASSIGNED_CONTEXT((#24538))
GLOBAL_UNIT_ASSIGNED_CONTEXT((#24629,#24631,#24632))
REPRESENTATION_CONTEXT('','3D')
) ;
#24587 = (
GEOMETRIC_REPRESENTATION_CONTEXT(3)
GLOBAL_UNCERTAINTY_ASSIGNED_CONTEXT((#24539))
GLOBAL_UNIT_ASSIGNED_CONTEXT((#24629,#24631,#24632))
REPRESENTATION_CONTEXT('','3D')
) ;
#24588 = (
GEOMETRIC_REPRESENTATION_CONTEXT(3)
GLOBAL_UNCERTAINTY_ASSIGNED_CONTEXT((#24540))
GLOBAL_UNIT_ASSIGNED_CONTEXT((#24629,#24631,#24632))
REPRESENTATION_CONTEXT('','3D')
) ;
#24589 = (
GEOMETRIC_REPRESENTATION_CONTEXT(3)
GLOBAL_UNCERTAINTY_ASSIGNED_CONTEXT((#24541))
GLOBAL_UNIT_ASSIGNED_CONTEXT((#24629,#24631,#24632))
REPRESENTATION_CONTEXT('','3D')
) ;
#24590 = (
GEOMETRIC_REPRESENTATION_CONTEXT(3)
GLOBAL_UNCERTAINTY_ASSIGNED_CONTEXT((#24542))
GLOBAL_UNIT_ASSIGNED_CONTEXT((#24629,#24631,#24632))
REPRESENTATION_CONTEXT('','3D')
) ;
#24591 = (
GEOMETRIC_REPRESENTATION_CONTEXT(3)
GLOBAL_UNCERTAINTY_ASSIGNED_CONTEXT((#24543))
GLOBAL_UNIT_ASSIGNED_CONTEXT((#24629,#24631,#24632))
REPRESENTATION_CONTEXT('','3D')
) ;
#24592 = (
GEOMETRIC_REPRESENTATION_CONTEXT(3)
GLOBAL_UNCERTAINTY_ASSIGNED_CONTEXT((#24544))
GLOBAL_UNIT_ASSIGNED_CONTEXT((#24629,#24631,#24632))
REPRESENTATION_CONTEXT('','3D')
) ;
#24593 = (
GEOMETRIC_REPRESENTATION_CONTEXT(3)
GLOBAL_UNCERTAINTY_ASSIGNED_CONTEXT((#24545))
GLOBAL_UNIT_ASSIGNED_CONTEXT((#24629,#24631,#24632))
REPRESENTATION_CONTEXT('','3D')
) ;
#24594 = (
GEOMETRIC_REPRESENTATION_CONTEXT(3)
GLOBAL_UNCERTAINTY_ASSIGNED_CONTEXT((#24546))
GLOBAL_UNIT_ASSIGNED_CONTEXT((#24629,#24631,#24632))
REPRESENTATION_CONTEXT('','3D')
) ;
#24595 = (
GEOMETRIC_REPRESENTATION_CONTEXT(3)
GLOBAL_UNCERTAINTY_ASSIGNED_CONTEXT((#24547))
GLOBAL_UNIT_ASSIGNED_CONTEXT((#24629,#24631,#24632))
REPRESENTATION_CONTEXT('','3D')
) ;
#24596 = (
GEOMETRIC_REPRESENTATION_CONTEXT(3)
GLOBAL_UNCERTAINTY_ASSIGNED_CONTEXT((#24548))
GLOBAL_UNIT_ASSIGNED_CONTEXT((#24629,#24631,#24632))
REPRESENTATION_CONTEXT('','3D')
) ;
#24597 = (
GEOMETRIC_REPRESENTATION_CONTEXT(3)
GLOBAL_UNCERTAINTY_ASSIGNED_CONTEXT((#24549))
GLOBAL_UNIT_ASSIGNED_CONTEXT((#24629,#24631,#24632))
REPRESENTATION_CONTEXT('','3D')
) ;
#24598 = (
GEOMETRIC_REPRESENTATION_CONTEXT(3)
GLOBAL_UNCERTAINTY_ASSIGNED_CONTEXT((#24550))
GLOBAL_UNIT_ASSIGNED_CONTEXT((#24629,#24631,#24632))
REPRESENTATION_CONTEXT('','3D')
) ;
#24599 = (
GEOMETRIC_REPRESENTATION_CONTEXT(3)
GLOBAL_UNCERTAINTY_ASSIGNED_CONTEXT((#24551))
GLOBAL_UNIT_ASSIGNED_CONTEXT((#24629,#24631,#24632))
REPRESENTATION_CONTEXT('','3D')
) ;
#24600 = (
GEOMETRIC_REPRESENTATION_CONTEXT(3)
GLOBAL_UNCERTAINTY_ASSIGNED_CONTEXT((#24552))
GLOBAL_UNIT_ASSIGNED_CONTEXT((#24629,#24631,#24632))
REPRESENTATION_CONTEXT('','3D')
) ;
#24601 = (
GEOMETRIC_REPRESENTATION_CONTEXT(3)
GLOBAL_UNCERTAINTY_ASSIGNED_CONTEXT((#24553))
GLOBAL_UNIT_ASSIGNED_CONTEXT((#24629,#24631,#24632))
REPRESENTATION_CONTEXT('','3D')
) ;
#24602 = (
GEOMETRIC_REPRESENTATION_CONTEXT(3)
GLOBAL_UNCERTAINTY_ASSIGNED_CONTEXT((#24554))
GLOBAL_UNIT_ASSIGNED_CONTEXT((#24629,#24631,#24632))
REPRESENTATION_CONTEXT('','3D')
) ;
#24603 = (
GEOMETRIC_REPRESENTATION_CONTEXT(3)
GLOBAL_UNCERTAINTY_ASSIGNED_CONTEXT((#24555))
GLOBAL_UNIT_ASSIGNED_CONTEXT((#24629,#24631,#24632))
REPRESENTATION_CONTEXT('','3D')
) ;
#24604 = (
GEOMETRIC_REPRESENTATION_CONTEXT(3)
GLOBAL_UNCERTAINTY_ASSIGNED_CONTEXT((#24556))
GLOBAL_UNIT_ASSIGNED_CONTEXT((#24629,#24631,#24632))
REPRESENTATION_CONTEXT('','3D')
) ;
#24605 = (
GEOMETRIC_REPRESENTATION_CONTEXT(3)
GLOBAL_UNCERTAINTY_ASSIGNED_CONTEXT((#24557))
GLOBAL_UNIT_ASSIGNED_CONTEXT((#24629,#24631,#24632))
REPRESENTATION_CONTEXT('','3D')
) ;
#24606 = (
GEOMETRIC_REPRESENTATION_CONTEXT(3)
GLOBAL_UNCERTAINTY_ASSIGNED_CONTEXT((#24558))
GLOBAL_UNIT_ASSIGNED_CONTEXT((#24629,#24631,#24632))
REPRESENTATION_CONTEXT('','3D')
) ;
#24607 = (
GEOMETRIC_REPRESENTATION_CONTEXT(3)
GLOBAL_UNCERTAINTY_ASSIGNED_CONTEXT((#24559))
GLOBAL_UNIT_ASSIGNED_CONTEXT((#24629,#24631,#24632))
REPRESENTATION_CONTEXT('','3D')
) ;
#24608 = (
GEOMETRIC_REPRESENTATION_CONTEXT(3)
GLOBAL_UNCERTAINTY_ASSIGNED_CONTEXT((#24560))
GLOBAL_UNIT_ASSIGNED_CONTEXT((#24629,#24631,#24632))
REPRESENTATION_CONTEXT('','3D')
) ;
#24609 = (
GEOMETRIC_REPRESENTATION_CONTEXT(3)
GLOBAL_UNCERTAINTY_ASSIGNED_CONTEXT((#24561))
GLOBAL_UNIT_ASSIGNED_CONTEXT((#24629,#24631,#24632))
REPRESENTATION_CONTEXT('','3D')
) ;
#24610 = (
GEOMETRIC_REPRESENTATION_CONTEXT(3)
GLOBAL_UNCERTAINTY_ASSIGNED_CONTEXT((#24562))
GLOBAL_UNIT_ASSIGNED_CONTEXT((#24629,#24631,#24632))
REPRESENTATION_CONTEXT('','3D')
) ;
#24611 = (
GEOMETRIC_REPRESENTATION_CONTEXT(3)
GLOBAL_UNCERTAINTY_ASSIGNED_CONTEXT((#24563))
GLOBAL_UNIT_ASSIGNED_CONTEXT((#24629,#24631,#24632))
REPRESENTATION_CONTEXT('','3D')
) ;
#24612 = (
GEOMETRIC_REPRESENTATION_CONTEXT(3)
GLOBAL_UNCERTAINTY_ASSIGNED_CONTEXT((#24564))
GLOBAL_UNIT_ASSIGNED_CONTEXT((#24629,#24631,#24632))
REPRESENTATION_CONTEXT('','3D')
) ;
#24613 = (
GEOMETRIC_REPRESENTATION_CONTEXT(3)
GLOBAL_UNCERTAINTY_ASSIGNED_CONTEXT((#24565))
GLOBAL_UNIT_ASSIGNED_CONTEXT((#24629,#24631,#24632))
REPRESENTATION_CONTEXT('','3D')
) ;
#24614 = (
GEOMETRIC_REPRESENTATION_CONTEXT(3)
GLOBAL_UNCERTAINTY_ASSIGNED_CONTEXT((#24566))
GLOBAL_UNIT_ASSIGNED_CONTEXT((#24629,#24631,#24632))
REPRESENTATION_CONTEXT('','3D')
) ;
#24615 = (
GEOMETRIC_REPRESENTATION_CONTEXT(3)
GLOBAL_UNCERTAINTY_ASSIGNED_CONTEXT((#24567))
GLOBAL_UNIT_ASSIGNED_CONTEXT((#24629,#24631,#24632))
REPRESENTATION_CONTEXT('','3D')
) ;
#24616 = (
GEOMETRIC_REPRESENTATION_CONTEXT(3)
GLOBAL_UNCERTAINTY_ASSIGNED_CONTEXT((#24568))
GLOBAL_UNIT_ASSIGNED_CONTEXT((#24629,#24631,#24632))
REPRESENTATION_CONTEXT('','3D')
) ;
#24617 = (
GEOMETRIC_REPRESENTATION_CONTEXT(3)
GLOBAL_UNCERTAINTY_ASSIGNED_CONTEXT((#24569))
GLOBAL_UNIT_ASSIGNED_CONTEXT((#24629,#24631,#24632))
REPRESENTATION_CONTEXT('','3D')
) ;
#24618 = (
GEOMETRIC_REPRESENTATION_CONTEXT(3)
GLOBAL_UNCERTAINTY_ASSIGNED_CONTEXT((#24570))
GLOBAL_UNIT_ASSIGNED_CONTEXT((#24629,#24631,#24632))
REPRESENTATION_CONTEXT('','3D')
) ;
#24619 = (
GEOMETRIC_REPRESENTATION_CONTEXT(3)
GLOBAL_UNCERTAINTY_ASSIGNED_CONTEXT((#24571))
GLOBAL_UNIT_ASSIGNED_CONTEXT((#24629,#24631,#24632))
REPRESENTATION_CONTEXT('','3D')
) ;
#24620 = (
GEOMETRIC_REPRESENTATION_CONTEXT(3)
GLOBAL_UNCERTAINTY_ASSIGNED_CONTEXT((#24572))
GLOBAL_UNIT_ASSIGNED_CONTEXT((#24629,#24631,#24632))
REPRESENTATION_CONTEXT('','3D')
) ;
#24621 = (
GEOMETRIC_REPRESENTATION_CONTEXT(3)
GLOBAL_UNCERTAINTY_ASSIGNED_CONTEXT((#24573))
GLOBAL_UNIT_ASSIGNED_CONTEXT((#24629,#24631,#24632))
REPRESENTATION_CONTEXT('','3D')
) ;
#24622 = (
GEOMETRIC_REPRESENTATION_CONTEXT(3)
GLOBAL_UNCERTAINTY_ASSIGNED_CONTEXT((#24574))
GLOBAL_UNIT_ASSIGNED_CONTEXT((#24629,#24631,#24632))
REPRESENTATION_CONTEXT('','3D')
) ;
#24623 = (
GEOMETRIC_REPRESENTATION_CONTEXT(3)
GLOBAL_UNCERTAINTY_ASSIGNED_CONTEXT((#24575))
GLOBAL_UNIT_ASSIGNED_CONTEXT((#24629,#24631,#24632))
REPRESENTATION_CONTEXT('','3D')
) ;
#24624 = (
GEOMETRIC_REPRESENTATION_CONTEXT(3)
GLOBAL_UNCERTAINTY_ASSIGNED_CONTEXT((#24576))
GLOBAL_UNIT_ASSIGNED_CONTEXT((#24629,#24631,#24632))
REPRESENTATION_CONTEXT('','3D')
) ;
#24625 = (
GEOMETRIC_REPRESENTATION_CONTEXT(3)
GLOBAL_UNCERTAINTY_ASSIGNED_CONTEXT((#24577))
GLOBAL_UNIT_ASSIGNED_CONTEXT((#24629,#24631,#24632))
REPRESENTATION_CONTEXT('','3D')
) ;
#24626 = (
GEOMETRIC_REPRESENTATION_CONTEXT(3)
GLOBAL_UNCERTAINTY_ASSIGNED_CONTEXT((#24578))
GLOBAL_UNIT_ASSIGNED_CONTEXT((#24629,#24631,#24632))
REPRESENTATION_CONTEXT('','3D')
) ;
#24627 = (
GEOMETRIC_REPRESENTATION_CONTEXT(3)
GLOBAL_UNCERTAINTY_ASSIGNED_CONTEXT((#24579))
GLOBAL_UNIT_ASSIGNED_CONTEXT((#24629,#24631,#24632))
REPRESENTATION_CONTEXT('','3D')
) ;
#24628 = (
GEOMETRIC_REPRESENTATION_CONTEXT(3)
GLOBAL_UNCERTAINTY_ASSIGNED_CONTEXT((#24580))
GLOBAL_UNIT_ASSIGNED_CONTEXT((#24629,#24631,#24632))
REPRESENTATION_CONTEXT('','3D')
) ;
#24629 = (
LENGTH_UNIT()
NAMED_UNIT(*)
SI_UNIT(.CENTI.,.METRE.)
) ;
#24630 = (
LENGTH_UNIT()
NAMED_UNIT(*)
SI_UNIT($,.METRE.)
) ;
#24631 = (
NAMED_UNIT(*)
PLANE_ANGLE_UNIT()
SI_UNIT($,.RADIAN.)
) ;
#24632 = (
NAMED_UNIT(*)
SI_UNIT($,.STERADIAN.)
SOLID_ANGLE_UNIT()
) ;
#24633 = SHAPE_DEFINITION_REPRESENTATION(#24680,#24791) ;
#24634 = SHAPE_DEFINITION_REPRESENTATION(#24681,#24792) ;
#24635 = SHAPE_DEFINITION_REPRESENTATION(#24682,#24793) ;
#24636 = SHAPE_DEFINITION_REPRESENTATION(#24683,#24794) ;
#24637 = SHAPE_DEFINITION_REPRESENTATION(#24684,#24795) ;
#24638 = SHAPE_DEFINITION_REPRESENTATION(#24685,#24796) ;
#24639 = SHAPE_DEFINITION_REPRESENTATION(#24686,#24797) ;
#24640 = SHAPE_DEFINITION_REPRESENTATION(#24687,#24798) ;
#24641 = SHAPE_DEFINITION_REPRESENTATION(#24688,#24799) ;
#24642 = SHAPE_DEFINITION_REPRESENTATION(#24689,#24800) ;
#24643 = SHAPE_DEFINITION_REPRESENTATION(#24690,#24801) ;
#24644 = SHAPE_DEFINITION_REPRESENTATION(#24691,#24802) ;
#24645 = SHAPE_DEFINITION_REPRESENTATION(#24692,#24803) ;
#24646 = SHAPE_DEFINITION_REPRESENTATION(#24693,#24804) ;
#24647 = SHAPE_DEFINITION_REPRESENTATION(#24694,#24805) ;
#24648 = SHAPE_DEFINITION_REPRESENTATION(#24695,#24806) ;
#24649 = SHAPE_DEFINITION_REPRESENTATION(#24696,#24807) ;
#24650 = SHAPE_DEFINITION_REPRESENTATION(#24697,#24808) ;
#24651 = SHAPE_DEFINITION_REPRESENTATION(#24698,#24809) ;
#24652 = SHAPE_DEFINITION_REPRESENTATION(#24699,#24810) ;
#24653 = SHAPE_DEFINITION_REPRESENTATION(#24700,#24811) ;
#24654 = SHAPE_DEFINITION_REPRESENTATION(#24723,#24812) ;
#24655 = SHAPE_DEFINITION_REPRESENTATION(#24724,#24813) ;
#24656 = SHAPE_DEFINITION_REPRESENTATION(#24725,#24814) ;
#24657 = SHAPE_DEFINITION_REPRESENTATION(#24726,#24815) ;
#24658 = SHAPE_DEFINITION_REPRESENTATION(#24727,#24816) ;
#24659 = SHAPE_DEFINITION_REPRESENTATION(#24728,#24817) ;
#24660 = SHAPE_DEFINITION_REPRESENTATION(#24729,#24818) ;
#24661 = SHAPE_DEFINITION_REPRESENTATION(#24730,#24819) ;
#24662 = SHAPE_DEFINITION_REPRESENTATION(#24731,#24820) ;
#24663 = SHAPE_DEFINITION_REPRESENTATION(#24732,#24821) ;
#24664 = SHAPE_DEFINITION_REPRESENTATION(#24733,#24822) ;
#24665 = SHAPE_DEFINITION_REPRESENTATION(#24734,#24823) ;
#24666 = SHAPE_DEFINITION_REPRESENTATION(#24747,#24824) ;
#24667 = SHAPE_DEFINITION_REPRESENTATION(#24748,#24825) ;
#24668 = SHAPE_DEFINITION_REPRESENTATION(#24749,#24826) ;
#24669 = SHAPE_DEFINITION_REPRESENTATION(#24750,#24827) ;
#24670 = SHAPE_DEFINITION_REPRESENTATION(#24751,#24828) ;
#24671 = SHAPE_DEFINITION_REPRESENTATION(#24752,#24829) ;
#24672 = SHAPE_DEFINITION_REPRESENTATION(#24753,#24830) ;
#24673 = SHAPE_DEFINITION_REPRESENTATION(#24761,#24831) ;
#24674 = SHAPE_DEFINITION_REPRESENTATION(#24762,#24832) ;
#24675 = SHAPE_DEFINITION_REPRESENTATION(#24763,#24833) ;
#24676 = SHAPE_DEFINITION_REPRESENTATION(#24764,#24834) ;
#24677 = SHAPE_DEFINITION_REPRESENTATION(#24765,#24835) ;
#24678 = SHAPE_DEFINITION_REPRESENTATION(#24766,#24836) ;
#24679 = SHAPE_DEFINITION_REPRESENTATION(#24767,#24837) ;
#24680 = PRODUCT_DEFINITION_SHAPE('',$,#24839) ;
#24681 = PRODUCT_DEFINITION_SHAPE('',$,#24840) ;
#24682 = PRODUCT_DEFINITION_SHAPE('',$,#24841) ;
#24683 = PRODUCT_DEFINITION_SHAPE('',$,#24842) ;
#24684 = PRODUCT_DEFINITION_SHAPE('',$,#24843) ;
#24685 = PRODUCT_DEFINITION_SHAPE('',$,#24844) ;
#24686 = PRODUCT_DEFINITION_SHAPE('',$,#24845) ;
#24687 = PRODUCT_DEFINITION_SHAPE('',$,#24846) ;
#24688 = PRODUCT_DEFINITION_SHAPE('',$,#24847) ;
#24689 = PRODUCT_DEFINITION_SHAPE('',$,#24848) ;
#24690 = PRODUCT_DEFINITION_SHAPE('',$,#24849) ;
#24691 = PRODUCT_DEFINITION_SHAPE('',$,#24850) ;
#24692 = PRODUCT_DEFINITION_SHAPE('',$,#24851) ;
#24693 = PRODUCT_DEFINITION_SHAPE('',$,#24852) ;
#24694 = PRODUCT_DEFINITION_SHAPE('',$,#24853) ;
#24695 = PRODUCT_DEFINITION_SHAPE('',$,#24854) ;
#24696 = PRODUCT_DEFINITION_SHAPE('',$,#24855) ;
#24697 = PRODUCT_DEFINITION_SHAPE('',$,#24856) ;
#24698 = PRODUCT_DEFINITION_SHAPE('',$,#24857) ;
#24699 = PRODUCT_DEFINITION_SHAPE('',$,#24858) ;
#24700 = PRODUCT_DEFINITION_SHAPE('',$,#24859) ;
#24701 = PRODUCT_DEFINITION_SHAPE($,$,#213) ;
#24702 = PRODUCT_DEFINITION_SHAPE($,$,#214) ;
#24703 = PRODUCT_DEFINITION_SHAPE($,$,#215) ;
#24704 = PRODUCT_DEFINITION_SHAPE($,$,#216) ;
#24705 = PRODUCT_DEFINITION_SHAPE($,$,#217) ;
#24706 = PRODUCT_DEFINITION_SHAPE($,$,#218) ;
#24707 = PRODUCT_DEFINITION_SHAPE($,$,#219) ;
#24708 = PRODUCT_DEFINITION_SHAPE($,$,#220) ;
#24709 = PRODUCT_DEFINITION_SHAPE($,$,#221) ;
#24710 = PRODUCT_DEFINITION_SHAPE($,$,#222) ;
#24711 = PRODUCT_DEFINITION_SHAPE($,$,#223) ;
#24712 = PRODUCT_DEFINITION_SHAPE($,$,#224) ;
#24713 = PRODUCT_DEFINITION_SHAPE($,$,#225) ;
#24714 = PRODUCT_DEFINITION_SHAPE($,$,#226) ;
#24715 = PRODUCT_DEFINITION_SHAPE($,$,#227) ;
#24716 = PRODUCT_DEFINITION_SHAPE($,$,#228) ;
#24717 = PRODUCT_DEFINITION_SHAPE($,$,#229) ;
#24718 = PRODUCT_DEFINITION_SHAPE($,$,#230) ;
#24719 = PRODUCT_DEFINITION_SHAPE($,$,#231) ;
#24720 = PRODUCT_DEFINITION_SHAPE($,$,#232) ;
#24721 = PRODUCT_DEFINITION_SHAPE($,$,#233) ;
#24722 = PRODUCT_DEFINITION_SHAPE($,$,#234) ;
#24723 = PRODUCT_DEFINITION_SHAPE('',$,#24860) ;
#24724 = PRODUCT_DEFINITION_SHAPE('',$,#24861) ;
#24725 = PRODUCT_DEFINITION_SHAPE('',$,#24862) ;
#24726 = PRODUCT_DEFINITION_SHAPE('',$,#24863) ;
#24727 = PRODUCT_DEFINITION_SHAPE('',$,#24864) ;
#24728 = PRODUCT_DEFINITION_SHAPE('',$,#24865) ;
#24729 = PRODUCT_DEFINITION_SHAPE('',$,#24866) ;
#24730 = PRODUCT_DEFINITION_SHAPE('',$,#24867) ;
#24731 = PRODUCT_DEFINITION_SHAPE('',$,#24868) ;
#24732 = PRODUCT_DEFINITION_SHAPE('',$,#24869) ;
#24733 = PRODUCT_DEFINITION_SHAPE('',$,#24870) ;
#24734 = PRODUCT_DEFINITION_SHAPE('',$,#24871) ;
#24735 = PRODUCT_DEFINITION_SHAPE($,$,#235) ;
#24736 = PRODUCT_DEFINITION_SHAPE($,$,#236) ;
#24737 = PRODUCT_DEFINITION_SHAPE($,$,#237) ;
#24738 = PRODUCT_DEFINITION_SHAPE($,$,#238) ;
#24739 = PRODUCT_DEFINITION_SHAPE($,$,#239) ;
#24740 = PRODUCT_DEFINITION_SHAPE($,$,#240) ;
#24741 = PRODUCT_DEFINITION_SHAPE($,$,#241) ;
#24742 = PRODUCT_DEFINITION_SHAPE($,$,#242) ;
#24743 = PRODUCT_DEFINITION_SHAPE($,$,#243) ;
#24744 = PRODUCT_DEFINITION_SHAPE($,$,#244) ;
#24745 = PRODUCT_DEFINITION_SHAPE($,$,#245) ;
#24746 = PRODUCT_DEFINITION_SHAPE($,$,#246) ;
#24747 = PRODUCT_DEFINITION_SHAPE('',$,#24872) ;
#24748 = PRODUCT_DEFINITION_SHAPE('',$,#24873) ;
#24749 = PRODUCT_DEFINITION_SHAPE('',$,#24874) ;
#24750 = PRODUCT_DEFINITION_SHAPE('',$,#24875) ;
#24751 = PRODUCT_DEFINITION_SHAPE('',$,#24876) ;
#24752 = PRODUCT_DEFINITION_SHAPE('',$,#24877) ;
#24753 = PRODUCT_DEFINITION_SHAPE('',$,#24878) ;
#24754 = PRODUCT_DEFINITION_SHAPE($,$,#247) ;
#24755 = PRODUCT_DEFINITION_SHAPE($,$,#248) ;
#24756 = PRODUCT_DEFINITION_SHAPE($,$,#249) ;
#24757 = PRODUCT_DEFINITION_SHAPE($,$,#250) ;
#24758 = PRODUCT_DEFINITION_SHAPE($,$,#251) ;
#24759 = PRODUCT_DEFINITION_SHAPE($,$,#252) ;
#24760 = PRODUCT_DEFINITION_SHAPE($,$,#253) ;
#24761 = PRODUCT_DEFINITION_SHAPE('',$,#24879) ;
#24762 = PRODUCT_DEFINITION_SHAPE('',$,#24880) ;
#24763 = PRODUCT_DEFINITION_SHAPE('',$,#24881) ;
#24764 = PRODUCT_DEFINITION_SHAPE('',$,#24882) ;
#24765 = PRODUCT_DEFINITION_SHAPE('',$,#24883) ;
#24766 = PRODUCT_DEFINITION_SHAPE('',$,#24884) ;
#24767 = PRODUCT_DEFINITION_SHAPE('',$,#24885) ;
#24768 = PRODUCT_DEFINITION_SHAPE($,$,#254) ;
#24769 = PRODUCT_DEFINITION_SHAPE($,$,#255) ;
#24770 = PRODUCT_DEFINITION_SHAPE($,$,#256) ;
#24771 = PRODUCT_DEFINITION_SHAPE($,$,#257) ;
#24772 = PRODUCT_DEFINITION_SHAPE($,$,#258) ;
#24773 = PRODUCT_DEFINITION_SHAPE($,$,#259) ;
#24774 = PRODUCT_DEFINITION_SHAPE($,$,#260) ;
#24775 = PRODUCT_DEFINITION_SHAPE($,$,#261) ;
#24776 = PRODUCT_DEFINITION_SHAPE($,$,#262) ;
#24777 = PRODUCT_DEFINITION_SHAPE($,$,#263) ;
#24778 = PRODUCT_DEFINITION_SHAPE($,$,#264) ;
#24779 = PRODUCT_DEFINITION_SHAPE($,$,#265) ;
#24780 = PRODUCT_DEFINITION_SHAPE($,$,#266) ;
#24781 = PRODUCT_DEFINITION_SHAPE($,$,#267) ;
#24782 = PRODUCT_DEFINITION_SHAPE($,$,#268) ;
#24783 = PRODUCT_DEFINITION_SHAPE($,$,#269) ;
#24784 = PRODUCT_DEFINITION_SHAPE($,$,#270) ;
#24785 = PRODUCT_DEFINITION_SHAPE($,$,#271) ;
#24786 = PRODUCT_DEFINITION_SHAPE($,$,#272) ;
#24787 = PRODUCT_DEFINITION_SHAPE($,$,#273) ;
#24788 = PRODUCT_DEFINITION_SHAPE($,$,#274) ;
#24789 = PRODUCT_DEFINITION_SHAPE($,$,#275) ;
#24790 = PRODUCT_DEFINITION_SHAPE($,$,#276) ;
#24791 = SHAPE_REPRESENTATION('',(#13652,#15386,#15387,#15388,#15389),#24581) ;
#24792 = SHAPE_REPRESENTATION('',(#13653,#14833,#14834,#14835,#14836,#14837,
#14838,#14839,#14840,#14841,#14842,#14843,#14844,#14845,#14846,#14847,#14848,
#14849,#14850,#14851,#14852,#14853,#14854),#24582) ;
#24793 = SHAPE_REPRESENTATION('',(#13654),#24583) ;
#24794 = SHAPE_REPRESENTATION('',(#13753),#24584) ;
#24795 = SHAPE_REPRESENTATION('',(#13805),#24585) ;
#24796 = SHAPE_REPRESENTATION('',(#13811),#24586) ;
#24797 = SHAPE_REPRESENTATION('',(#13838),#24587) ;
#24798 = SHAPE_REPRESENTATION('',(#13875),#24588) ;
#24799 = SHAPE_REPRESENTATION('',(#14061),#24589) ;
#24800 = SHAPE_REPRESENTATION('',(#14078),#24590) ;
#24801 = SHAPE_REPRESENTATION('',(#14095),#24591) ;
#24802 = SHAPE_REPRESENTATION('',(#14104),#24592) ;
#24803 = SHAPE_REPRESENTATION('',(#14115),#24593) ;
#24804 = SHAPE_REPRESENTATION('',(#14200),#24594) ;
#24805 = SHAPE_REPRESENTATION('',(#14207),#24595) ;
#24806 = SHAPE_REPRESENTATION('',(#14216),#24596) ;
#24807 = SHAPE_REPRESENTATION('',(#14227),#24597) ;
#24808 = SHAPE_REPRESENTATION('',(#14253),#24598) ;
#24809 = SHAPE_REPRESENTATION('',(#14259),#24599) ;
#24810 = SHAPE_REPRESENTATION('',(#14495),#24600) ;
#24811 = SHAPE_REPRESENTATION('',(#14802),#24601) ;
#24812 = SHAPE_REPRESENTATION('',(#14855,#15169,#15170,#15171,#15172,#15173,
#15174,#15175,#15176,#15177,#15178,#15179,#15180),#24602) ;
#24813 = SHAPE_REPRESENTATION('',(#14856),#24603) ;
#24814 = SHAPE_REPRESENTATION('',(#14863),#24604) ;
#24815 = SHAPE_REPRESENTATION('',(#14884),#24605) ;
#24816 = SHAPE_REPRESENTATION('',(#14939),#24606) ;
#24817 = SHAPE_REPRESENTATION('',(#14993),#24607) ;
#24818 = SHAPE_REPRESENTATION('',(#14999),#24608) ;
#24819 = SHAPE_REPRESENTATION('',(#15008),#24609) ;
#24820 = SHAPE_REPRESENTATION('',(#15093),#24610) ;
#24821 = SHAPE_REPRESENTATION('',(#15102),#24611) ;
#24822 = SHAPE_REPRESENTATION('',(#15143),#24612) ;
#24823 = SHAPE_REPRESENTATION('',(#15156),#24613) ;
#24824 = SHAPE_REPRESENTATION('',(#15181,#15290,#15291,#15292,#15293,#15294,
#15295,#15296),#24614) ;
#24825 = SHAPE_REPRESENTATION('',(#15182),#24615) ;
#24826 = SHAPE_REPRESENTATION('',(#15192),#24616) ;
#24827 = SHAPE_REPRESENTATION('',(#15213),#24617) ;
#24828 = SHAPE_REPRESENTATION('',(#15222),#24618) ;
#24829 = SHAPE_REPRESENTATION('',(#15243),#24619) ;
#24830 = SHAPE_REPRESENTATION('',(#15264),#24620) ;
#24831 = SHAPE_REPRESENTATION('',(#15297,#15367,#15368,#15369,#15370,#15371,
#15372,#15373,#15374,#15375,#15376,#15377,#15378,#15379,#15380,#15381,#15382,
#15383,#15384,#15385),#24621) ;
#24832 = SHAPE_REPRESENTATION('',(#15298),#24622) ;
#24833 = SHAPE_REPRESENTATION('',(#15308),#24623) ;
#24834 = SHAPE_REPRESENTATION('',(#15317),#24624) ;
#24835 = SHAPE_REPRESENTATION('',(#15329),#24625) ;
#24836 = SHAPE_REPRESENTATION('',(#15342),#24626) ;
#24837 = SHAPE_REPRESENTATION('',(#15355),#24627) ;
#24838 = PRODUCT_DEFINITION_CONTEXT('part definition',#24981,'design') ;
#24839 = PRODUCT_DEFINITION('BR-648',
'BR-648',#24886,#24838) ;
#24840 = PRODUCT_DEFINITION('CORE_METERING_UNIT',
'CORE_METERING_UNIT',#24887,#24838) ;
#24841 = PRODUCT_DEFINITION('REAR_SHELL_ENCLOSURE',
'REAR_SHELL_ENCLOSURE',#24888,#24838) ;
#24842 = PRODUCT_DEFINITION('FRONT_SHELL_ENCLOSURE',
'FRONT_SHELL_ENCLOSURE',#24889,#24838) ;
#24843 = PRODUCT_DEFINITION('INSPECTION_WINDOW','INSPECTION_WINDOW',
#24890,#24838) ;
#24844 = PRODUCT_DEFINITION('SHELL_SEAL_GASKET','SHELL_SEAL_GASKET',
#24891,#24838) ;
#24845 = PRODUCT_DEFINITION('CENTRAL_AXIS_SHAFT',
'CENTRAL_AXIS_SHAFT',#24892,#24838) ;
#24846 = PRODUCT_DEFINITION('ROTATING_SEEDING_PLATE',
'ROTATING_SEEDING_PLATE',#24893,#24838) ;
#24847 = PRODUCT_DEFINITION('SEALED_ROLLER_BEARING_6202_OUTER',
'SEALED_ROLLER_BEARING_6202_OUTER',#24894,#24838) ;
#24848 = PRODUCT_DEFINITION('SEALED_ROLLER_BEARING_6202_INNER',
'SEALED_ROLLER_BEARING_6202_INNER',#24895,#24838) ;
#24849 = PRODUCT_DEFINITION('BEARING_SPACER_SLEEVE',
'BEARING_SPACER_SLEEVE',#24896,#24838) ;
#24850 = PRODUCT_DEFINITION('SHAFT_RETAINING_CIRCLIP',
'SHAFT_RETAINING_CIRCLIP',#24897,#24838) ;
#24851 = PRODUCT_DEFINITION('DRIVE_SPROCKET_12T',
'DRIVE_SPROCKET_12T',#24898,#24838) ;
#24852 = PRODUCT_DEFINITION('PARALLEL_KEY_5x5','PARALLEL_KEY_5x5',
#24899,#24838) ;
#24853 = PRODUCT_DEFINITION('INTERNAL_SEED_PROTECTION_BOARD',
'INTERNAL_SEED_PROTECTION_BOARD',#24900,#24838) ;
#24854 = PRODUCT_DEFINITION('PERIPHERAL_DISPENSER_BUCKET',
'PERIPHERAL_DISPENSER_BUCKET',#24901,#24838) ;
#24855 = PRODUCT_DEFINITION('SPRING_LOADED_EJECTOR_ARM',
'SPRING_LOADED_EJECTOR_ARM',#24902,#24838) ;
#24856 = PRODUCT_DEFINITION('EJECTOR_PIVOT_PIN','EJECTOR_PIVOT_PIN',
#24903,#24838) ;
#24857 = PRODUCT_DEFINITION('EJECTOR_TORSION_SPRING',
'EJECTOR_TORSION_SPRING',#24904,#24838) ;
#24858 = PRODUCT_DEFINITION('EXTERNAL_SPIRAL_RETURN_PIPE',
'EXTERNAL_SPIRAL_RETURN_PIPE',#24905,#24838) ;
#24859 = PRODUCT_DEFINITION('MOUNTING_BRACKET_FLANGE',
'MOUNTING_BRACKET_FLANGE',#24906,#24838) ;
#24860 = PRODUCT_DEFINITION('SEED_FEED_HOPPER_UNIT',
'SEED_FEED_HOPPER_UNIT',#24907,#24838) ;
#24861 = PRODUCT_DEFINITION('SEED_FEED_HOPPER','SEED_FEED_HOPPER',
#24908,#24838) ;
#24862 = PRODUCT_DEFINITION('HOPPER_LID','HOPPER_LID',#24909,
#24838) ;
#24863 = PRODUCT_DEFINITION('FEED_ROLLER_HOUSING',
'FEED_ROLLER_HOUSING',#24910,#24838) ;
#24864 = PRODUCT_DEFINITION('FLUTED_FEED_ROLLER',
'FLUTED_FEED_ROLLER',#24911,#24838) ;
#24865 = PRODUCT_DEFINITION('FEED_ROLLER_SHAFT','FEED_ROLLER_SHAFT',
#24912,#24838) ;
#24866 = PRODUCT_DEFINITION('FEED_ROLLER_BUSHING',
'FEED_ROLLER_BUSHING',#24913,#24838) ;
#24867 = PRODUCT_DEFINITION('FEED_ROLLER_SPROCKET',
'FEED_ROLLER_SPROCKET',#24914,#24838) ;
#24868 = PRODUCT_DEFINITION('HOPPER_DISCHARGE_SPOUT',
'HOPPER_DISCHARGE_SPOUT',#24915,#24838) ;
#24869 = PRODUCT_DEFINITION('SEED_FEED_HOSE','SEED_FEED_HOSE',#24916,
#24838) ;
#24870 = PRODUCT_DEFINITION('HOSE_CLAMP_WORM_DRIVE',
'HOSE_CLAMP_WORM_DRIVE',#24917,#24838) ;
#24871 = PRODUCT_DEFINITION('HOSE_CLAMP_WORM_DRIVE_2',
'HOSE_CLAMP_WORM_DRIVE_2',#24918,#24838) ;
#24872 = PRODUCT_DEFINITION('VENTURI_UNIT','VENTURI_UNIT',#24919,
#24838) ;
#24873 = PRODUCT_DEFINITION('VENTURI_TUBE','VENTURI_TUBE',#24920,
#24838) ;
#24874 = PRODUCT_DEFINITION('VENTURI_THROAT_INSERT',
'VENTURI_THROAT_INSERT',#24921,#24838) ;
#24875 = PRODUCT_DEFINITION('SEED_DROP_SPOUT','SEED_DROP_SPOUT',#24922,
#24838) ;
#24876 = PRODUCT_DEFINITION('VENTURI_AIR_INLET_FLANGE',
'VENTURI_AIR_INLET_FLANGE',#24923,#24838) ;
#24877 = PRODUCT_DEFINITION('VENTURI_OUTLET_FLANGE',
'VENTURI_OUTLET_FLANGE',#24924,#24838) ;
#24878 = PRODUCT_DEFINITION('VENTURI_SADDLE_CLAMP',
'VENTURI_SADDLE_CLAMP',#24925,#24838) ;
#24879 = PRODUCT_DEFINITION('FASTENERS','FASTENERS',#24926,
#24838) ;
#24880 = PRODUCT_DEFINITION('HUB_SCREW_M4','HUB_SCREW_M4',#24927,
#24838) ;
#24881 = PRODUCT_DEFINITION('HUB_LOCK_WASHER','HUB_LOCK_WASHER',#24928,
#24838) ;
#24882 = PRODUCT_DEFINITION('HUB_LOCK_NUT_M10','HUB_LOCK_NUT_M10',
#24929,#24838) ;
#24883 = PRODUCT_DEFINITION('BRACKET_BOLT_M8x16',
'BRACKET_BOLT_M8x16',#24930,#24838) ;
#24884 = PRODUCT_DEFINITION('SHELL_CLAMP_BOLT_M6x85',
'SHELL_CLAMP_BOLT_M6x85',#24931,#24838) ;
#24885 = PRODUCT_DEFINITION('SHELL_CLAMP_NUT_M6',
'SHELL_CLAMP_NUT_M6',#24932,#24838) ;
#24886 = PRODUCT_DEFINITION_FORMATION('',$,#24983) ;
#24887 = PRODUCT_DEFINITION_FORMATION('',$,#24984) ;
#24888 = PRODUCT_DEFINITION_FORMATION('',$,#24985) ;
#24889 = PRODUCT_DEFINITION_FORMATION('',$,#24986) ;
#24890 = PRODUCT_DEFINITION_FORMATION('',$,#24987) ;
#24891 = PRODUCT_DEFINITION_FORMATION('',$,#24988) ;
#24892 = PRODUCT_DEFINITION_FORMATION('',$,#24989) ;
#24893 = PRODUCT_DEFINITION_FORMATION('',$,#24990) ;
#24894 = PRODUCT_DEFINITION_FORMATION('',$,#24991) ;
#24895 = PRODUCT_DEFINITION_FORMATION('',$,#24992) ;
#24896 = PRODUCT_DEFINITION_FORMATION('',$,#24993) ;
#24897 = PRODUCT_DEFINITION_FORMATION('',$,#24994) ;
#24898 = PRODUCT_DEFINITION_FORMATION('',$,#24995) ;
#24899 = PRODUCT_DEFINITION_FORMATION('',$,#24996) ;
#24900 = PRODUCT_DEFINITION_FORMATION('',$,#24997) ;
#24901 = PRODUCT_DEFINITION_FORMATION('',$,#24998) ;
#24902 = PRODUCT_DEFINITION_FORMATION('',$,#24999) ;
#24903 = PRODUCT_DEFINITION_FORMATION('',$,#25000) ;
#24904 = PRODUCT_DEFINITION_FORMATION('',$,#25001) ;
#24905 = PRODUCT_DEFINITION_FORMATION('',$,#25002) ;
#24906 = PRODUCT_DEFINITION_FORMATION('',$,#25003) ;
#24907 = PRODUCT_DEFINITION_FORMATION('',$,#25004) ;
#24908 = PRODUCT_DEFINITION_FORMATION('',$,#25005) ;
#24909 = PRODUCT_DEFINITION_FORMATION('',$,#25006) ;
#24910 = PRODUCT_DEFINITION_FORMATION('',$,#25007) ;
#24911 = PRODUCT_DEFINITION_FORMATION('',$,#25008) ;
#24912 = PRODUCT_DEFINITION_FORMATION('',$,#25009) ;
#24913 = PRODUCT_DEFINITION_FORMATION('',$,#25010) ;
#24914 = PRODUCT_DEFINITION_FORMATION('',$,#25011) ;
#24915 = PRODUCT_DEFINITION_FORMATION('',$,#25012) ;
#24916 = PRODUCT_DEFINITION_FORMATION('',$,#25013) ;
#24917 = PRODUCT_DEFINITION_FORMATION('',$,#25014) ;
#24918 = PRODUCT_DEFINITION_FORMATION('',$,#25015) ;
#24919 = PRODUCT_DEFINITION_FORMATION('',$,#25016) ;
#24920 = PRODUCT_DEFINITION_FORMATION('',$,#25017) ;
#24921 = PRODUCT_DEFINITION_FORMATION('',$,#25018) ;
#24922 = PRODUCT_DEFINITION_FORMATION('',$,#25019) ;
#24923 = PRODUCT_DEFINITION_FORMATION('',$,#25020) ;
#24924 = PRODUCT_DEFINITION_FORMATION('',$,#25021) ;
#24925 = PRODUCT_DEFINITION_FORMATION('',$,#25022) ;
#24926 = PRODUCT_DEFINITION_FORMATION('',$,#25023) ;
#24927 = PRODUCT_DEFINITION_FORMATION('',$,#25024) ;
#24928 = PRODUCT_DEFINITION_FORMATION('',$,#25025) ;
#24929 = PRODUCT_DEFINITION_FORMATION('',$,#25026) ;
#24930 = PRODUCT_DEFINITION_FORMATION('',$,#25027) ;
#24931 = PRODUCT_DEFINITION_FORMATION('',$,#25028) ;
#24932 = PRODUCT_DEFINITION_FORMATION('',$,#25029) ;
#24933 = PRODUCT_RELATED_PRODUCT_CATEGORY('BR-648',
'BR-648',(#24983)) ;
#24934 = PRODUCT_RELATED_PRODUCT_CATEGORY('CORE_METERING_UNIT',
'CORE_METERING_UNIT',(#24984)) ;
#24935 = PRODUCT_RELATED_PRODUCT_CATEGORY('REAR_SHELL_ENCLOSURE',
'REAR_SHELL_ENCLOSURE',(#24985)) ;
#24936 = PRODUCT_RELATED_PRODUCT_CATEGORY('FRONT_SHELL_ENCLOSURE',
'FRONT_SHELL_ENCLOSURE',(#24986)) ;
#24937 = PRODUCT_RELATED_PRODUCT_CATEGORY('INSPECTION_WINDOW',
'INSPECTION_WINDOW',(#24987)) ;
#24938 = PRODUCT_RELATED_PRODUCT_CATEGORY('SHELL_SEAL_GASKET',
'SHELL_SEAL_GASKET',(#24988)) ;
#24939 = PRODUCT_RELATED_PRODUCT_CATEGORY('CENTRAL_AXIS_SHAFT',
'CENTRAL_AXIS_SHAFT',(#24989)) ;
#24940 = PRODUCT_RELATED_PRODUCT_CATEGORY('ROTATING_SEEDING_PLATE',
'ROTATING_SEEDING_PLATE',(#24990)) ;
#24941 = PRODUCT_RELATED_PRODUCT_CATEGORY(
'SEALED_ROLLER_BEARING_6202_OUTER','SEALED_ROLLER_BEARING_6202_OUTER',(#24991)) ;
#24942 = PRODUCT_RELATED_PRODUCT_CATEGORY(
'SEALED_ROLLER_BEARING_6202_INNER','SEALED_ROLLER_BEARING_6202_INNER',(#24992)) ;
#24943 = PRODUCT_RELATED_PRODUCT_CATEGORY('BEARING_SPACER_SLEEVE',
'BEARING_SPACER_SLEEVE',(#24993)) ;
#24944 = PRODUCT_RELATED_PRODUCT_CATEGORY('SHAFT_RETAINING_CIRCLIP',
'SHAFT_RETAINING_CIRCLIP',(#24994)) ;
#24945 = PRODUCT_RELATED_PRODUCT_CATEGORY('DRIVE_SPROCKET_12T',
'DRIVE_SPROCKET_12T',(#24995)) ;
#24946 = PRODUCT_RELATED_PRODUCT_CATEGORY('PARALLEL_KEY_5x5',
'PARALLEL_KEY_5x5',(#24996)) ;
#24947 = PRODUCT_RELATED_PRODUCT_CATEGORY(
'INTERNAL_SEED_PROTECTION_BOARD','INTERNAL_SEED_PROTECTION_BOARD',(#24997)) ;
#24948 = PRODUCT_RELATED_PRODUCT_CATEGORY('PERIPHERAL_DISPENSER_BUCKET',
'PERIPHERAL_DISPENSER_BUCKET',(#24998)) ;
#24949 = PRODUCT_RELATED_PRODUCT_CATEGORY('SPRING_LOADED_EJECTOR_ARM',
'SPRING_LOADED_EJECTOR_ARM',(#24999)) ;
#24950 = PRODUCT_RELATED_PRODUCT_CATEGORY('EJECTOR_PIVOT_PIN',
'EJECTOR_PIVOT_PIN',(#25000)) ;
#24951 = PRODUCT_RELATED_PRODUCT_CATEGORY('EJECTOR_TORSION_SPRING',
'EJECTOR_TORSION_SPRING',(#25001)) ;
#24952 = PRODUCT_RELATED_PRODUCT_CATEGORY('EXTERNAL_SPIRAL_RETURN_PIPE',
'EXTERNAL_SPIRAL_RETURN_PIPE',(#25002)) ;
#24953 = PRODUCT_RELATED_PRODUCT_CATEGORY('MOUNTING_BRACKET_FLANGE',
'MOUNTING_BRACKET_FLANGE',(#25003)) ;
#24954 = PRODUCT_RELATED_PRODUCT_CATEGORY('SEED_FEED_HOPPER_UNIT',
'SEED_FEED_HOPPER_UNIT',(#25004)) ;
#24955 = PRODUCT_RELATED_PRODUCT_CATEGORY('SEED_FEED_HOPPER',
'SEED_FEED_HOPPER',(#25005)) ;
#24956 = PRODUCT_RELATED_PRODUCT_CATEGORY('HOPPER_LID','HOPPER_LID',(#25006)) ;
#24957 = PRODUCT_RELATED_PRODUCT_CATEGORY('FEED_ROLLER_HOUSING',
'FEED_ROLLER_HOUSING',(#25007)) ;
#24958 = PRODUCT_RELATED_PRODUCT_CATEGORY('FLUTED_FEED_ROLLER',
'FLUTED_FEED_ROLLER',(#25008)) ;
#24959 = PRODUCT_RELATED_PRODUCT_CATEGORY('FEED_ROLLER_SHAFT',
'FEED_ROLLER_SHAFT',(#25009)) ;
#24960 = PRODUCT_RELATED_PRODUCT_CATEGORY('FEED_ROLLER_BUSHING',
'FEED_ROLLER_BUSHING',(#25010)) ;
#24961 = PRODUCT_RELATED_PRODUCT_CATEGORY('FEED_ROLLER_SPROCKET',
'FEED_ROLLER_SPROCKET',(#25011)) ;
#24962 = PRODUCT_RELATED_PRODUCT_CATEGORY('HOPPER_DISCHARGE_SPOUT',
'HOPPER_DISCHARGE_SPOUT',(#25012)) ;
#24963 = PRODUCT_RELATED_PRODUCT_CATEGORY('SEED_FEED_HOSE',
'SEED_FEED_HOSE',(#25013)) ;
#24964 = PRODUCT_RELATED_PRODUCT_CATEGORY('HOSE_CLAMP_WORM_DRIVE',
'HOSE_CLAMP_WORM_DRIVE',(#25014)) ;
#24965 = PRODUCT_RELATED_PRODUCT_CATEGORY('HOSE_CLAMP_WORM_DRIVE_2',
'HOSE_CLAMP_WORM_DRIVE_2',(#25015)) ;
#24966 = PRODUCT_RELATED_PRODUCT_CATEGORY('VENTURI_UNIT','VENTURI_UNIT',(#25016)) ;
#24967 = PRODUCT_RELATED_PRODUCT_CATEGORY('VENTURI_TUBE','VENTURI_TUBE',(#25017)) ;
#24968 = PRODUCT_RELATED_PRODUCT_CATEGORY('VENTURI_THROAT_INSERT',
'VENTURI_THROAT_INSERT',(#25018)) ;
#24969 = PRODUCT_RELATED_PRODUCT_CATEGORY('SEED_DROP_SPOUT',
'SEED_DROP_SPOUT',(#25019)) ;
#24970 = PRODUCT_RELATED_PRODUCT_CATEGORY('VENTURI_AIR_INLET_FLANGE',
'VENTURI_AIR_INLET_FLANGE',(#25020)) ;
#24971 = PRODUCT_RELATED_PRODUCT_CATEGORY('VENTURI_OUTLET_FLANGE',
'VENTURI_OUTLET_FLANGE',(#25021)) ;
#24972 = PRODUCT_RELATED_PRODUCT_CATEGORY('VENTURI_SADDLE_CLAMP',
'VENTURI_SADDLE_CLAMP',(#25022)) ;
#24973 = PRODUCT_RELATED_PRODUCT_CATEGORY('FASTENERS','FASTENERS',(#25023)) ;
#24974 = PRODUCT_RELATED_PRODUCT_CATEGORY('HUB_SCREW_M4','HUB_SCREW_M4',(#25024)) ;
#24975 = PRODUCT_RELATED_PRODUCT_CATEGORY('HUB_LOCK_WASHER',
'HUB_LOCK_WASHER',(#25025)) ;
#24976 = PRODUCT_RELATED_PRODUCT_CATEGORY('HUB_LOCK_NUT_M10',
'HUB_LOCK_NUT_M10',(#25026)) ;
#24977 = PRODUCT_RELATED_PRODUCT_CATEGORY('BRACKET_BOLT_M8x16',
'BRACKET_BOLT_M8x16',(#25027)) ;
#24978 = PRODUCT_RELATED_PRODUCT_CATEGORY('SHELL_CLAMP_BOLT_M6x85',
'SHELL_CLAMP_BOLT_M6x85',(#25028)) ;
#24979 = PRODUCT_RELATED_PRODUCT_CATEGORY('SHELL_CLAMP_NUT_M6',
'SHELL_CLAMP_NUT_M6',(#25029)) ;
#24980 = APPLICATION_PROTOCOL_DEFINITION('international standard',
'automotive_design',2009,#24981) ;
#24981 = APPLICATION_CONTEXT(
'Core Data for Automotive Mechanical Design Process') ;
#24982 = PRODUCT_CONTEXT('part definition',#24981,'mechanical') ;
#24983 = PRODUCT('BR-648','BR-648',
$,(#24982)) ;
#24984 = PRODUCT('CORE_METERING_UNIT','CORE_METERING_UNIT',$,(#24982)) ;
#24985 = PRODUCT('REAR_SHELL_ENCLOSURE','REAR_SHELL_ENCLOSURE',$,(#24982)) ;
#24986 = PRODUCT('FRONT_SHELL_ENCLOSURE','FRONT_SHELL_ENCLOSURE',$,(#24982)) ;
#24987 = PRODUCT('INSPECTION_WINDOW','INSPECTION_WINDOW',$,(#24982)) ;
#24988 = PRODUCT('SHELL_SEAL_GASKET','SHELL_SEAL_GASKET',$,(#24982)) ;
#24989 = PRODUCT('CENTRAL_AXIS_SHAFT','CENTRAL_AXIS_SHAFT',$,(#24982)) ;
#24990 = PRODUCT('ROTATING_SEEDING_PLATE','ROTATING_SEEDING_PLATE',$,(#24982)) ;
#24991 = PRODUCT('SEALED_ROLLER_BEARING_6202_OUTER',
'SEALED_ROLLER_BEARING_6202_OUTER',$,(#24982)) ;
#24992 = PRODUCT('SEALED_ROLLER_BEARING_6202_INNER',
'SEALED_ROLLER_BEARING_6202_INNER',$,(#24982)) ;
#24993 = PRODUCT('BEARING_SPACER_SLEEVE','BEARING_SPACER_SLEEVE',$,(#24982)) ;
#24994 = PRODUCT('SHAFT_RETAINING_CIRCLIP','SHAFT_RETAINING_CIRCLIP',$,(#24982)) ;
#24995 = PRODUCT('DRIVE_SPROCKET_12T','DRIVE_SPROCKET_12T',$,(#24982)) ;
#24996 = PRODUCT('PARALLEL_KEY_5x5','PARALLEL_KEY_5x5',$,(#24982)) ;
#24997 = PRODUCT('INTERNAL_SEED_PROTECTION_BOARD',
'INTERNAL_SEED_PROTECTION_BOARD',$,(#24982)) ;
#24998 = PRODUCT('PERIPHERAL_DISPENSER_BUCKET','PERIPHERAL_DISPENSER_BUCKET',
$,(#24982)) ;
#24999 = PRODUCT('SPRING_LOADED_EJECTOR_ARM','SPRING_LOADED_EJECTOR_ARM',$,
(#24982)) ;
#25000 = PRODUCT('EJECTOR_PIVOT_PIN','EJECTOR_PIVOT_PIN',$,(#24982)) ;
#25001 = PRODUCT('EJECTOR_TORSION_SPRING','EJECTOR_TORSION_SPRING',$,(#24982)) ;
#25002 = PRODUCT('EXTERNAL_SPIRAL_RETURN_PIPE','EXTERNAL_SPIRAL_RETURN_PIPE',
$,(#24982)) ;
#25003 = PRODUCT('MOUNTING_BRACKET_FLANGE','MOUNTING_BRACKET_FLANGE',$,(#24982)) ;
#25004 = PRODUCT('SEED_FEED_HOPPER_UNIT','SEED_FEED_HOPPER_UNIT',$,(#24982)) ;
#25005 = PRODUCT('SEED_FEED_HOPPER','SEED_FEED_HOPPER',$,(#24982)) ;
#25006 = PRODUCT('HOPPER_LID','HOPPER_LID',$,(#24982)) ;
#25007 = PRODUCT('FEED_ROLLER_HOUSING','FEED_ROLLER_HOUSING',$,(#24982)) ;
#25008 = PRODUCT('FLUTED_FEED_ROLLER','FLUTED_FEED_ROLLER',$,(#24982)) ;
#25009 = PRODUCT('FEED_ROLLER_SHAFT','FEED_ROLLER_SHAFT',$,(#24982)) ;
#25010 = PRODUCT('FEED_ROLLER_BUSHING','FEED_ROLLER_BUSHING',$,(#24982)) ;
#25011 = PRODUCT('FEED_ROLLER_SPROCKET','FEED_ROLLER_SPROCKET',$,(#24982)) ;
#25012 = PRODUCT('HOPPER_DISCHARGE_SPOUT','HOPPER_DISCHARGE_SPOUT',$,(#24982)) ;
#25013 = PRODUCT('SEED_FEED_HOSE','SEED_FEED_HOSE',$,(#24982)) ;
#25014 = PRODUCT('HOSE_CLAMP_WORM_DRIVE','HOSE_CLAMP_WORM_DRIVE',$,(#24982)) ;
#25015 = PRODUCT('HOSE_CLAMP_WORM_DRIVE_2','HOSE_CLAMP_WORM_DRIVE_2',$,(#24982)) ;
#25016 = PRODUCT('VENTURI_UNIT','VENTURI_UNIT',$,(#24982)) ;
#25017 = PRODUCT('VENTURI_TUBE','VENTURI_TUBE',$,(#24982)) ;
#25018 = PRODUCT('VENTURI_THROAT_INSERT','VENTURI_THROAT_INSERT',$,(#24982)) ;
#25019 = PRODUCT('SEED_DROP_SPOUT','SEED_DROP_SPOUT',$,(#24982)) ;
#25020 = PRODUCT('VENTURI_AIR_INLET_FLANGE','VENTURI_AIR_INLET_FLANGE',$,(#24982)) ;
#25021 = PRODUCT('VENTURI_OUTLET_FLANGE','VENTURI_OUTLET_FLANGE',$,(#24982)) ;
#25022 = PRODUCT('VENTURI_SADDLE_CLAMP','VENTURI_SADDLE_CLAMP',$,(#24982)) ;
#25023 = PRODUCT('FASTENERS','FASTENERS',$,(#24982)) ;
#25024 = PRODUCT('HUB_SCREW_M4','HUB_SCREW_M4',$,(#24982)) ;
#25025 = PRODUCT('HUB_LOCK_WASHER','HUB_LOCK_WASHER',$,(#24982)) ;
#25026 = PRODUCT('HUB_LOCK_NUT_M10','HUB_LOCK_NUT_M10',$,(#24982)) ;
#25027 = PRODUCT('BRACKET_BOLT_M8x16','BRACKET_BOLT_M8x16',$,(#24982)) ;
#25028 = PRODUCT('SHELL_CLAMP_BOLT_M6x85','SHELL_CLAMP_BOLT_M6x85',$,(#24982)) ;
#25029 = PRODUCT('SHELL_CLAMP_NUT_M6','SHELL_CLAMP_NUT_M6',$,(#24982)) ;
#25030 = PRESENTATION_STYLE_ASSIGNMENT((#25040)) ;
#25031 = PRESENTATION_STYLE_ASSIGNMENT((#25041)) ;
#25032 = PRESENTATION_STYLE_ASSIGNMENT((#25042)) ;
#25033 = PRESENTATION_STYLE_ASSIGNMENT((#25043)) ;
#25034 = PRESENTATION_STYLE_ASSIGNMENT((#25044)) ;
#25035 = PRESENTATION_STYLE_ASSIGNMENT((#25045)) ;
#25036 = PRESENTATION_STYLE_ASSIGNMENT((#25046)) ;
#25037 = PRESENTATION_STYLE_ASSIGNMENT((#25047)) ;
#25038 = PRESENTATION_STYLE_ASSIGNMENT((#25048)) ;
#25039 = PRESENTATION_STYLE_ASSIGNMENT((#25049)) ;
#25040 = SURFACE_STYLE_USAGE(.BOTH.,#25050) ;
#25041 = SURFACE_STYLE_USAGE(.BOTH.,#25051) ;
#25042 = SURFACE_STYLE_USAGE(.BOTH.,#25052) ;
#25043 = SURFACE_STYLE_USAGE(.BOTH.,#25053) ;
#25044 = SURFACE_STYLE_USAGE(.BOTH.,#25054) ;
#25045 = SURFACE_STYLE_USAGE(.BOTH.,#25055) ;
#25046 = SURFACE_STYLE_USAGE(.BOTH.,#25056) ;
#25047 = SURFACE_STYLE_USAGE(.BOTH.,#25057) ;
#25048 = SURFACE_STYLE_USAGE(.BOTH.,#25058) ;
#25049 = SURFACE_STYLE_USAGE(.BOTH.,#25059) ;
#25050 = SURFACE_SIDE_STYLE('',(#25060)) ;
#25051 = SURFACE_SIDE_STYLE('',(#25061)) ;
#25052 = SURFACE_SIDE_STYLE('',(#25062)) ;
#25053 = SURFACE_SIDE_STYLE('',(#25063)) ;
#25054 = SURFACE_SIDE_STYLE('',(#25064)) ;
#25055 = SURFACE_SIDE_STYLE('',(#25065)) ;
#25056 = SURFACE_SIDE_STYLE('',(#25066)) ;
#25057 = SURFACE_SIDE_STYLE('',(#25067)) ;
#25058 = SURFACE_SIDE_STYLE('',(#25068)) ;
#25059 = SURFACE_SIDE_STYLE('',(#25069)) ;
#25060 = SURFACE_STYLE_FILL_AREA(#25070) ;
#25061 = SURFACE_STYLE_FILL_AREA(#25071) ;
#25062 = SURFACE_STYLE_FILL_AREA(#25072) ;
#25063 = SURFACE_STYLE_FILL_AREA(#25073) ;
#25064 = SURFACE_STYLE_FILL_AREA(#25074) ;
#25065 = SURFACE_STYLE_FILL_AREA(#25075) ;
#25066 = SURFACE_STYLE_FILL_AREA(#25076) ;
#25067 = SURFACE_STYLE_FILL_AREA(#25077) ;
#25068 = SURFACE_STYLE_FILL_AREA(#25078) ;
#25069 = SURFACE_STYLE_FILL_AREA(#25079) ;
#25070 = FILL_AREA_STYLE('Steel - Satin',(#25080)) ;
#25071 = FILL_AREA_STYLE('Aluminum - Satin',(#25081)) ;
#25072 = FILL_AREA_STYLE('Plastic - Glossy (Grey)',(#25082)) ;
#25073 = FILL_AREA_STYLE('Rubber - Soft',(#25083)) ;
#25074 = FILL_AREA_STYLE('Stainless Steel - Satin',(#25084)) ;
#25075 = FILL_AREA_STYLE('ABS (White)',(#25085)) ;
#25076 = FILL_AREA_STYLE('Nylon 6-6 (White)',(#25086)) ;
#25077 = FILL_AREA_STYLE('Steel - Galvanized (Small)',(#25087)) ;
#25078 = FILL_AREA_STYLE('Surface - Matte',(#25088)) ;
#25079 = FILL_AREA_STYLE('Brass - Polished',(#25089)) ;
#25080 = FILL_AREA_STYLE_COLOUR('Steel - Satin',#25090) ;
#25081 = FILL_AREA_STYLE_COLOUR('Aluminum - Satin',#25091) ;
#25082 = FILL_AREA_STYLE_COLOUR('Plastic - Glossy (Grey)',#25092) ;
#25083 = FILL_AREA_STYLE_COLOUR('Rubber - Soft',#25093) ;
#25084 = FILL_AREA_STYLE_COLOUR('Stainless Steel - Satin',#25094) ;
#25085 = FILL_AREA_STYLE_COLOUR('ABS (White)',#25095) ;
#25086 = FILL_AREA_STYLE_COLOUR('Nylon 6-6 (White)',#25096) ;
#25087 = FILL_AREA_STYLE_COLOUR('Steel - Galvanized (Small)',#25097) ;
#25088 = FILL_AREA_STYLE_COLOUR('Surface - Matte',#25098) ;
#25089 = FILL_AREA_STYLE_COLOUR('Brass - Polished',#25099) ;
#25090 = COLOUR_RGB('Steel - Satin', 0.66274510, 0.83137255, 0.94901961) ;
#25091 = COLOUR_RGB('Aluminum - Satin', 0.40784314, 0.44705882, 0.49803922) ;
#25092 = COLOUR_RGB('Plastic - Glossy (Grey)', 0.08235294, 0.09019608, 0.10196078) ;
#25093 = COLOUR_RGB('Rubber - Soft', 0.09019608, 0.27058824, 0.51372549) ;
#25094 = COLOUR_RGB('Stainless Steel - Satin', 0.31764706, 0.68627451, 0.89019608) ;
#25095 = COLOUR_RGB('ABS (White)', 0.66274510, 0.83137255, 0.94901961) ;
#25096 = COLOUR_RGB('Nylon 6-6 (White)', 0.31764706, 0.68627451, 0.89019608) ;
#25097 = COLOUR_RGB('Steel - Galvanized (Small)', 0.31764706, 0.68627451, 0.89019608) ;
#25098 = COLOUR_RGB('Surface - Matte', 0.66274510, 0.83137255, 0.94901961) ;
#25099 = COLOUR_RGB('Brass - Polished', 0.09019608, 0.27058824, 0.51372549) ;
ENDSEC;
END-ISO-10303-21;
